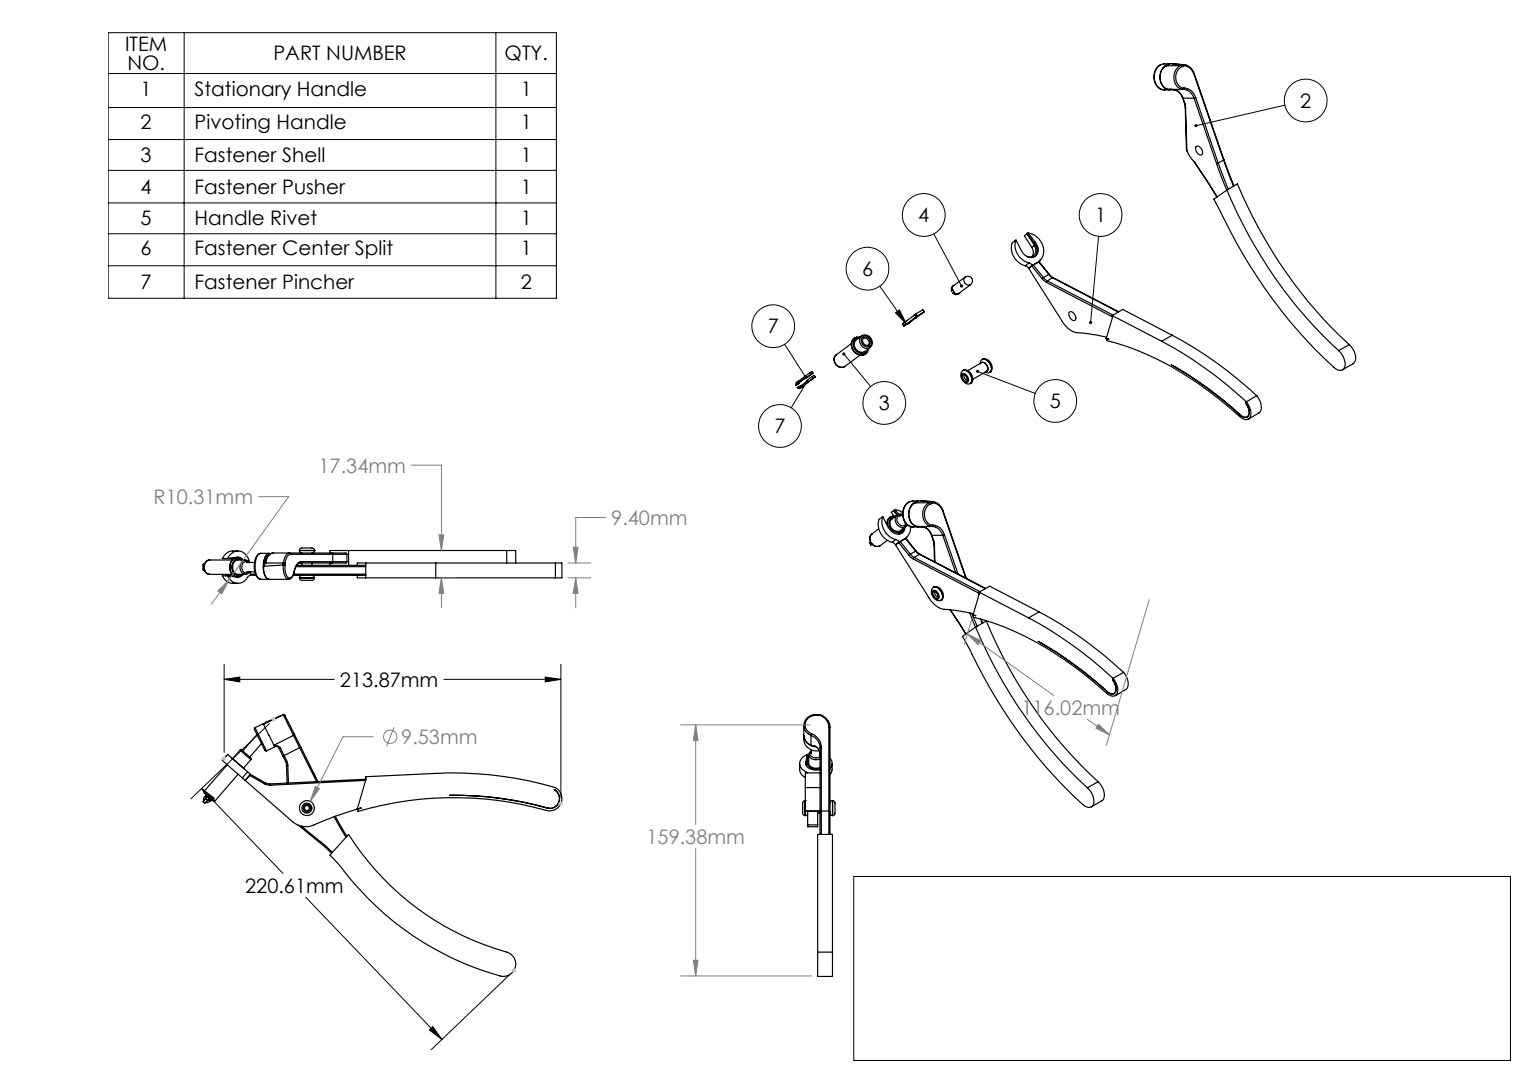
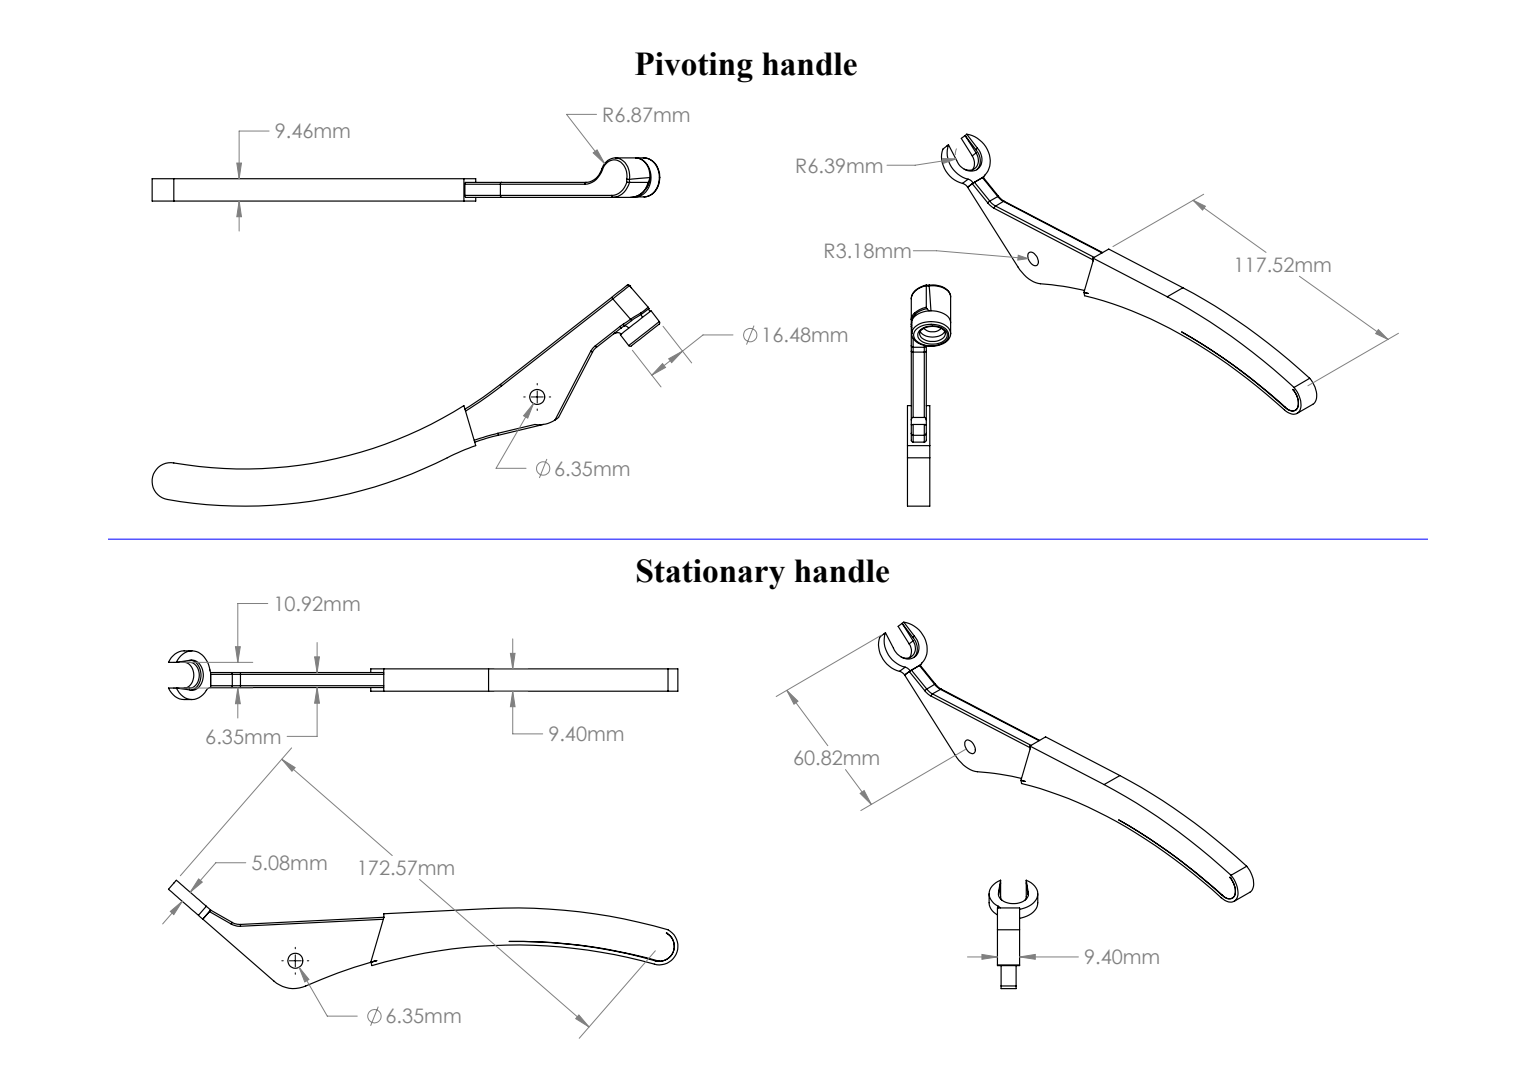
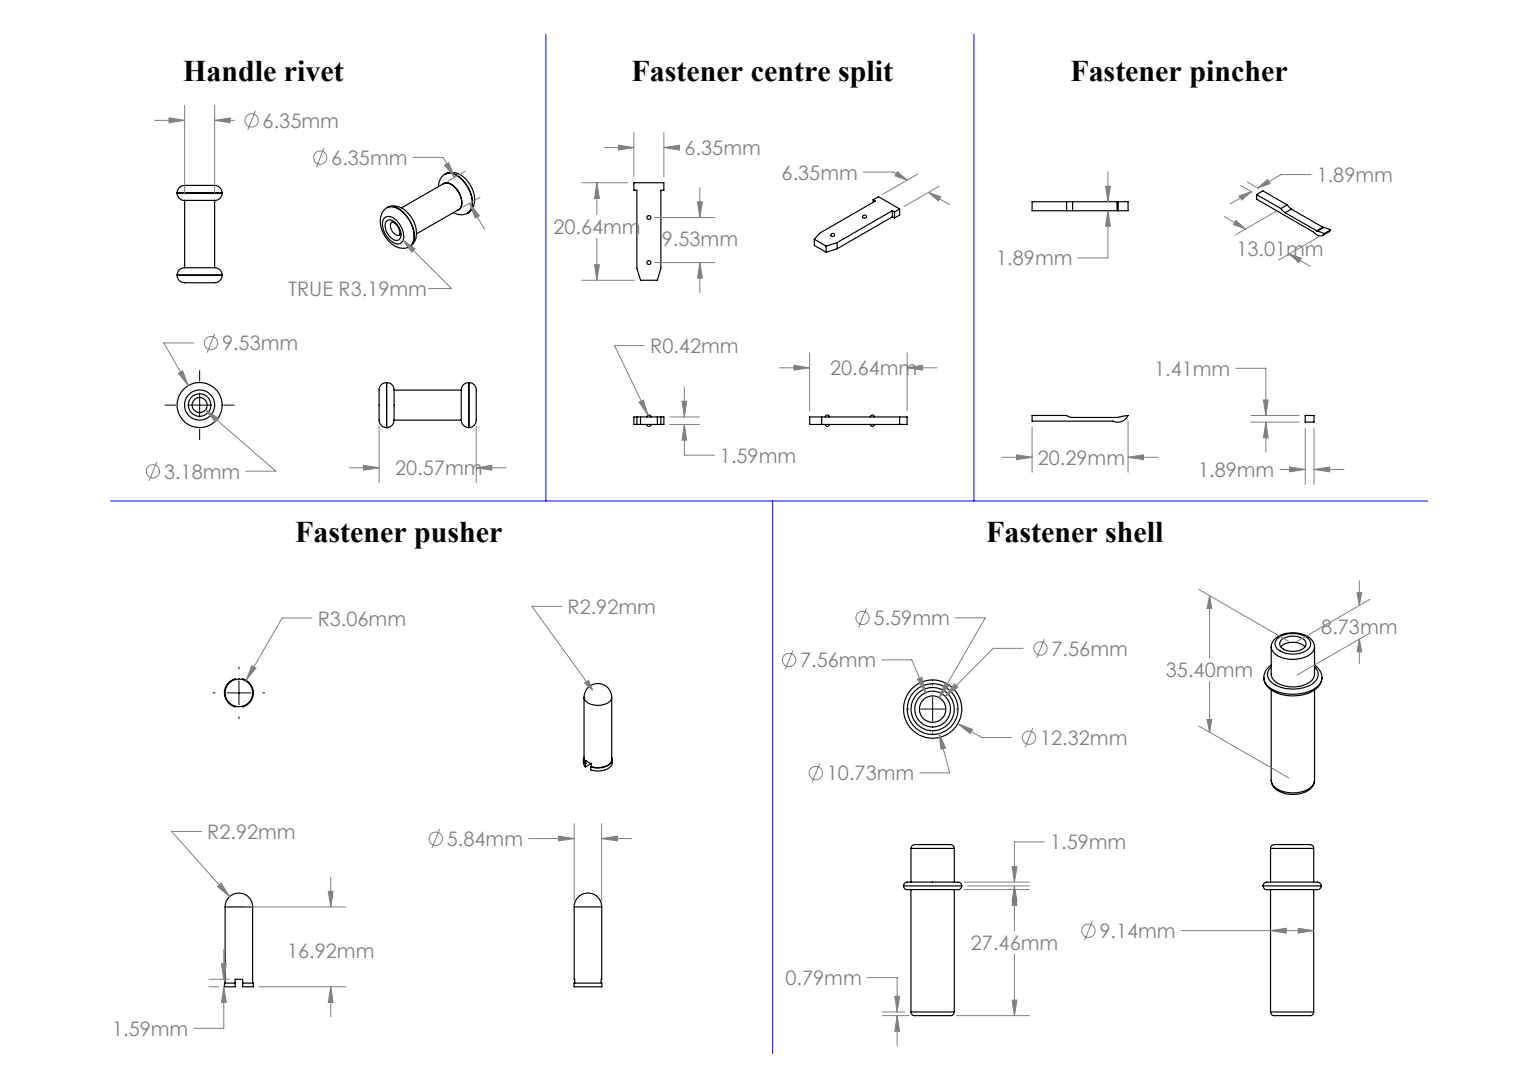
ISO-10303-21;
HEADER;
FILE_DESCRIPTION (('STEP AP203'),
    '1' );
FILE_NAME ('MAS-157',
    '2026-10-09T13:45:32',
    ( '' ),
    ( '' ),
    'SwSTEP 2.0',
    'SolidWorks 2024',
    '' );
FILE_SCHEMA (( 'AUTOMOTIVE_DESIGN' ));
ENDSEC;

DATA;
#1 = DIRECTION ( 'NONE',  ( -0.6157549048526801405, 0.7879377495398142139, 0.000000000000000000 ) ) ;
#2 = SHAPE_REPRESENTATION ( 'Cleco, Handle, Stationary', ( #3555 ), #5783 ) ;
#3 = DIRECTION ( 'NONE',  ( -1.000000000000000000, 0.000000000000000000, 0.000000000000000000 ) ) ;
#4 = ORIENTED_EDGE ( 'NONE', *, *, #5907, .T. ) ;
#5 = CARTESIAN_POINT ( 'NONE',  ( 1.850068364776406682, 1.494658567734585608, 0.000000000000000000 ) ) ;
#6 = VERTEX_POINT ( 'NONE', #7280 ) ;
#7 = LINE ( 'NONE', #8071, #3494 ) ;
#8 = PERSON_AND_ORGANIZATION ( #4735, #6190 ) ;
#9 = CARTESIAN_POINT ( 'NONE',  ( -5.996547682996108186, -1.882193845889704065, 0.2179999999999999993 ) ) ;
#10 = FACE_OUTER_BOUND ( 'NONE', #4917, .T. ) ;
#11 = EDGE_CURVE ( 'NONE', #2855, #2155, #1899, .T. ) ;
#12 = ORIENTED_EDGE ( 'NONE', *, *, #4444, .T. ) ;
#13 = FACE_OUTER_BOUND ( 'NONE', #2691, .T. ) ;
#14 = CARTESIAN_POINT ( 'NONE',  ( 0.6250000000000000000, -0.07812500000000001388, 0.000000000000000000 ) ) ;
#15 = DIRECTION ( 'NONE',  ( 1.000000000000000000, 8.970601940444434686E-12, 0.000000000000000000 ) ) ;
#16 = APPROVAL_DATE_TIME ( #593, #3996 ) ;
#17 = LINE ( 'NONE', #7477, #1803 ) ;
#18 = DIRECTION ( 'NONE',  ( 0.000000000000000000, 0.000000000000000000, -1.000000000000000000 ) ) ;
#19 = VERTEX_POINT ( 'NONE', #3930 ) ;
#20 = ORIENTED_EDGE ( 'NONE', *, *, #5646, .T. ) ;
#21 = EDGE_CURVE ( 'NONE', #2327, #24, #2891, .T. ) ;
#22 = EDGE_CURVE ( 'NONE', #963, #158, #1365, .T. ) ;
#23 = LOCAL_TIME ( 14, 45, 32.00000000000000000, #7946 ) ;
#24 = VERTEX_POINT ( 'NONE', #7323 ) ;
#25 = AXIS2_PLACEMENT_3D ( 'NONE', #111, #2600, #7606 ) ;
#26 = FACE_OUTER_BOUND ( 'NONE', #6824, .T. ) ;
#27 = CC_DESIGN_PERSON_AND_ORGANIZATION_ASSIGNMENT ( #2008, #749, ( #3335 ) ) ;
#28 = CARTESIAN_POINT ( 'NONE',  ( 1.416570667224800406, 1.056400084382879134, -0.2054632529226294024 ) ) ;
#29 = EDGE_CURVE ( 'NONE', #3273, #1544, #5158, .T. ) ;
#30 = LINE ( 'NONE', #3883, #1333 ) ;
#31 = ORIENTED_EDGE ( 'NONE', *, *, #3836, .F. ) ;
#32 = DIRECTION ( 'NONE',  ( -0.000000000000000000, 0.000000000000000000, 1.000000000000000000 ) ) ;
#33 = B_SPLINE_CURVE_WITH_KNOTS ( 'NONE', 3,
 ( #1903, #1397, #3941, #5831 ),
 .UNSPECIFIED., .F., .F.,
 ( 4, 4 ),
 ( 0.001688628934469491114, 0.002127673841090521080 ),
 .UNSPECIFIED. ) ;
#34 = VECTOR ( 'NONE', #5125, 39.37007874015748143 ) ;
#35 = CARTESIAN_POINT ( 'NONE',  ( -1.204376266962890796, -0.2040480809676099017, 0.2500000000000000000 ) ) ;
#36 = CARTESIAN_POINT ( 'NONE',  ( -1.763177565995708296, 1.070083551578370207, -0.08100000000000007194 ) ) ;
#37 = CALENDAR_DATE ( 2026, 9, 10 ) ;
#38 = ORIENTED_EDGE ( 'NONE', *, *, #6492, .T. ) ;
#39 = CIRCLE ( 'NONE', #5286, 0.06200000000000004813 ) ;
#40 = CARTESIAN_POINT ( 'NONE',  ( 1.323792169463187340, 1.088966521967518863, -0.1270528182937126493 ) ) ;
#41 = CARTESIAN_POINT ( 'NONE',  ( 0.000000000000000000, 0.6124999999999999334, 0.000000000000000000 ) ) ;
#42 = CARTESIAN_POINT ( 'NONE',  ( 1.684866161243239846, 1.178252195112418299, -0.1039999999999998703 ) ) ;
#43 = VECTOR ( 'NONE', #928, 39.37007874015748143 ) ;
#44 = CARTESIAN_POINT ( 'NONE',  ( -1.067641779222573639, 0.6107141540073635078, 0.09374999999999998612 ) ) ;
#45 = DIRECTION ( 'NONE',  ( 1.000000000000000000, 0.000000000000000000, 0.000000000000000000 ) ) ;
#46 = DIRECTION ( 'NONE',  ( -0.000000000000000000, -0.000000000000000000, -1.000000000000000000 ) ) ;
#47 = CARTESIAN_POINT ( 'NONE',  ( 0.000000000000000000, 0.6124999999999999334, 0.000000000000000000 ) ) ;
#48 = CIRCLE ( 'NONE', #181, 0.3547681700190749576 ) ;
#49 = AXIS2_PLACEMENT_3D ( 'NONE', #6623, #1014, #5431 ) ;
#50 = ORIENTED_EDGE ( 'NONE', *, *, #1216, .T. ) ;
#51 = SECURITY_CLASSIFICATION ( '', '', #1852 ) ;
#52 = CIRCLE ( 'NONE', #6609, 0.1875000000000000278 ) ;
#53 = EDGE_LOOP ( 'NONE', ( #7030, #861, #647, #7343 ) ) ;
#54 = DIRECTION ( 'NONE',  ( -0.000000000000000000, -0.000000000000000000, -1.000000000000000000 ) ) ;
#55 = DIRECTION ( 'NONE',  ( -1.000000000000000000, 0.000000000000000000, 0.000000000000000000 ) ) ;
#56 = MECHANICAL_CONTEXT ( 'NONE', #1115, 'mechanical' ) ;
#57 = CARTESIAN_POINT ( 'NONE',  ( 6.190221022838899856, 0.4584861219976859026, 0.1250000000000004441 ) ) ;
#58 = FACE_BOUND ( 'NONE', #2776, .T. ) ;
#59 = ORIENTED_EDGE ( 'NONE', *, *, #2335, .F. ) ;
#60 = VECTOR ( 'NONE', #178, 39.37007874015747433 ) ;
#61 = AXIS2_PLACEMENT_3D ( 'NONE', #3635, #4900, #4323 ) ;
#62 = DIRECTION ( 'NONE',  ( 0.8639477456102231390, 0.5035814659566147933, -0.000000000000000000 ) ) ;
#63 = CIRCLE ( 'NONE', #3353, 0.09999999999999999167 ) ;
#64 = CIRCLE ( 'NONE', #588, 0.1255000000000000282 ) ;
#65 = ORIENTED_EDGE ( 'NONE', *, *, #5052, .T. ) ;
#66 = FACE_OUTER_BOUND ( 'NONE', #5233, .T. ) ;
#67 = CYLINDRICAL_SURFACE ( 'NONE', #6771, 0.03124999999999999306 ) ;
#68 = EDGE_CURVE ( 'NONE', #5482, #3124, #1464, .T. ) ;
#69 = EDGE_CURVE ( 'NONE', #6638, #4615, #2677, .T. ) ;
#70 = CARTESIAN_POINT ( 'NONE',  ( 1.752412446118922995, 1.417229020394738415, 0.1726873346618605365 ) ) ;
#71 = ORIENTED_EDGE ( 'NONE', *, *, #7527, .T. ) ;
#72 = DIRECTION ( 'NONE',  ( 0.000000000000000000, 0.000000000000000000, -1.000000000000000000 ) ) ;
#73 = CIRCLE ( 'NONE', #5578, 0.2425000000000000211 ) ;
#74 = EDGE_CURVE ( 'NONE', #1061, #1984, #3077, .T. ) ;
#75 = ORIENTED_EDGE ( 'NONE', *, *, #993, .T. ) ;
#76 = FACE_OUTER_BOUND ( 'NONE', #4236, .T. ) ;
#77 = DIRECTION ( 'NONE',  ( -1.000000000000000000, 0.000000000000000000, 0.000000000000000000 ) ) ;
#78 = AXIS2_PLACEMENT_3D ( 'NONE', #1308, #3818, #6319 ) ;
#79 = APPLICATION_PROTOCOL_DEFINITION ( 'international standard', 'config_control_design', 1994, #1637 ) ;
#80 = EDGE_CURVE ( 'NONE', #1875, #4512, #6627, .T. ) ;
#81 = VERTEX_POINT ( 'NONE', #6665 ) ;
#82 = EDGE_CURVE ( 'NONE', #7062, #4072, #1053, .T. ) ;
#83 = DIRECTION ( 'NONE',  ( 0.000000000000000000, 0.000000000000000000, 1.000000000000000000 ) ) ;
#84 = DIRECTION ( 'NONE',  ( 0.7879377495398138809, 0.6157549048526804736, 0.000000000000000000 ) ) ;
#85 = EDGE_LOOP ( 'NONE', ( #926, #3795, #4009, #2620 ) ) ;
#86 = AXIS2_PLACEMENT_3D ( 'NONE', #7852, #2824, #5333 ) ;
#87 = DIRECTION ( 'NONE',  ( -0.6568496200222107007, -0.7540216022612863389, 0.000000000000000000 ) ) ;
#88 = AXIS2_PLACEMENT_3D ( 'NONE', #2138, #3280, #7015 ) ;
#89 = APPROVAL ( #7734, 'UNSPECIFIED' ) ;
#90 = EDGE_CURVE ( 'NONE', #3501, #7797, #7679, .T. ) ;
#91 = VERTEX_POINT ( 'NONE', #2513 ) ;
#92 = AXIS2_PLACEMENT_3D ( 'NONE', #7571, #6383, #766 ) ;
#93 = DIRECTION ( 'NONE',  ( 0.7879377495398159903, 0.6157549048526775870, -0.000000000000000000 ) ) ;
#94 = APPROVAL_ROLE ( '' ) ;
#95 = DIRECTION ( 'NONE',  ( 0.000000000000000000, 1.000000000000000000, 0.000000000000000000 ) ) ;
#96 = DATE_AND_TIME ( #5751, #4257 ) ;
#97 = CARTESIAN_POINT ( 'NONE',  ( 0.000000000000000000, 0.03124999999999997571, 0.000000000000000000 ) ) ;
#98 = CIRCLE ( 'NONE', #4156, 6.962657474112426748 ) ;
#99 = ORIENTED_EDGE ( 'NONE', *, *, #6424, .F. ) ;
#100 = AXIS2_PLACEMENT_3D ( 'NONE', #6028, #4066, #402 ) ;
#101 = FACE_OUTER_BOUND ( 'NONE', #53, .T. ) ;
#102 = PERSON_AND_ORGANIZATION ( #4735, #6190 ) ;
#103 = CARTESIAN_POINT ( 'NONE',  ( -0.1250000000000000000, 1.530808498934191509E-17, -0.5599999999999999423 ) ) ;
#104 = DIRECTION ( 'NONE',  ( 1.821231995776175479E-16, 1.000000000000000000, 0.000000000000000000 ) ) ;
#105 = ORIENTED_EDGE ( 'NONE', *, *, #272, .F. ) ;
#106 = ORIENTED_EDGE ( 'NONE', *, *, #2026, .T. ) ;
#107 = FACE_OUTER_BOUND ( 'NONE', #1359, .T. ) ;
#108 = ORIENTED_EDGE ( 'NONE', *, *, #7591, .T. ) ;
#109 = CARTESIAN_POINT ( 'NONE',  ( 0.000000000000000000, 0.000000000000000000, 0.2500000000000000000 ) ) ;
#110 = CARTESIAN_POINT ( 'NONE',  ( 1.417684048173985634, 1.054372030571947283, -0.2033754655707550874 ) ) ;
#111 = CARTESIAN_POINT ( 'NONE',  ( 0.000000000000000000, 0.000000000000000000, 0.2500000000000000000 ) ) ;
#112 = VERTEX_POINT ( 'NONE', #7478 ) ;
#113 = DIRECTION ( 'NONE',  ( 0.000000000000000000, 0.000000000000000000, -1.000000000000000000 ) ) ;
#114 = ORIENTED_EDGE ( 'NONE', *, *, #7639, .F. ) ;
#115 = CARTESIAN_POINT ( 'NONE',  ( 1.832772415705825830, 1.448773774648827617, 0.06821617062301892076 ) ) ;
#116 = DIRECTION ( 'NONE',  ( 1.000000000000000000, -0.000000000000000000, -0.000000000000000000 ) ) ;
#117 = DATE_AND_TIME ( #5742, #3955 ) ;
#118 = ORIENTED_EDGE ( 'NONE', *, *, #4536, .T. ) ;
#119 = DIRECTION ( 'NONE',  ( 0.000000000000000000, 0.000000000000000000, -1.000000000000000000 ) ) ;
#120 = CARTESIAN_POINT ( 'NONE',  ( 1.380988422957101003, 1.174934410393058126, 0.2179999999999999993 ) ) ;
#121 = ORIENTED_EDGE ( 'NONE', *, *, #1777, .F. ) ;
#122 = DIRECTION ( 'NONE',  ( 0.7540216022612864499, -0.6568496200222104786, 0.000000000000000000 ) ) ;
#123 = EDGE_CURVE ( 'NONE', #4974, #3239, #3718, .T. ) ;
#124 = ADVANCED_FACE ( 'NONE', ( #549 ), #7584, .F. ) ;
#125 = EDGE_CURVE ( 'NONE', #2487, #1575, #5560, .T. ) ;
#126 = EDGE_CURVE ( 'NONE', #3812, #6, #587, .T. ) ;
#127 =( CONVERSION_BASED_UNIT ( 'INCH', #2499 ) LENGTH_UNIT ( ) NAMED_UNIT ( #5631 ) );
#128 = DIRECTION ( 'NONE',  ( -0.000000000000000000, 1.000000000000000000, -0.000000000000000000 ) ) ;
#129 = ORIENTED_EDGE ( 'NONE', *, *, #6348, .F. ) ;
#130 = CARTESIAN_POINT ( 'NONE',  ( 1.531818848064314453, 1.858671604592519344, -3.087930470258342319E-05 ) ) ;
#131 = EDGE_CURVE ( 'NONE', #668, #4233, #6788, .T. ) ;
#132 = DIRECTION ( 'NONE',  ( 0.000000000000000000, 0.000000000000000000, 1.000000000000000000 ) ) ;
#133 = EDGE_CURVE ( 'NONE', #2990, #3476, #3761, .T. ) ;
#134 = ORIENTED_EDGE ( 'NONE', *, *, #3394, .F. ) ;
#135 = DIRECTION ( 'NONE',  ( 1.000000000000000000, 0.000000000000000000, 0.000000000000000000 ) ) ;
#136 = CARTESIAN_POINT ( 'NONE',  ( 1.723350842796532278, 1.129006085766179890, -0.1039999999999998703 ) ) ;
#137 = COORDINATED_UNIVERSAL_TIME_OFFSET ( 0, 0, .AHEAD. ) ;
#138 = DIRECTION ( 'NONE',  ( -0.4606913525677313603, -0.8875604078987042733, -0.000000000000000000 ) ) ;
#139 = DIRECTION ( 'NONE',  ( -0.000000000000000000, 0.000000000000000000, 1.000000000000000000 ) ) ;
#140 = VERTEX_POINT ( 'NONE', #3018 ) ;
#141 = VERTEX_POINT ( 'NONE', #7361 ) ;
#142 = EDGE_LOOP ( 'NONE', ( #3147, #7500, #5095 ) ) ;
#143 = FACE_OUTER_BOUND ( 'NONE', #230, .T. ) ;
#144 = APPROVAL_PERSON_ORGANIZATION ( #7760, #2585, #5389 ) ;
#145 = EDGE_LOOP ( 'NONE', ( #637, #5534, #4273, #3035, #377, #5498, #741, #1949, #1567, #4620 ) ) ;
#146 = DIRECTION ( 'NONE',  ( -0.04906492035527518919, 0.9987955914953422498, 0.000000000000000000 ) ) ;
#147 = CARTESIAN_POINT ( 'NONE',  ( 0.2896281645421511231, -0.04777128394798136474, 0.07449999999999999678 ) ) ;
#148 = CARTESIAN_POINT ( 'NONE',  ( -0.1250000000000000000, 0.5625000000000000000, 0.03125000000000000000 ) ) ;
#149 = CARTESIAN_POINT ( 'NONE',  ( 0.1250000000000000000, 0.000000000000000000, -0.5599999999999999423 ) ) ;
#150 = LOCAL_TIME ( 14, 45, 32.00000000000000000, #1109 ) ;
#151 = EDGE_LOOP ( 'NONE', ( #4432, #6165, #5491, #6432 ) ) ;
#152 = CARTESIAN_POINT ( 'NONE',  ( 1.792094459600980905, 1.446946837835136890, 0.1263687957420392971 ) ) ;
#153 = DIRECTION ( 'NONE',  ( -0.000000000000000000, -1.000000000000000000, -0.000000000000000000 ) ) ;
#154 = PERSON_AND_ORGANIZATION ( #4735, #6190 ) ;
#155 = ORIENTED_EDGE ( 'NONE', *, *, #2026, .F. ) ;
#156 = CARTESIAN_POINT ( 'NONE',  ( -4.882388066182508091, 5.670153330992292240, 0.000000000000000000 ) ) ;
#157 = FACE_OUTER_BOUND ( 'NONE', #262, .T. ) ;
#158 = VERTEX_POINT ( 'NONE', #6270 ) ;
#159 = CIRCLE ( 'NONE', #7494, 0.1255000000000000282 ) ;
#160 = FACE_OUTER_BOUND ( 'NONE', #466, .T. ) ;
#161 = AXIS2_PLACEMENT_3D ( 'NONE', #1394, #5055, #7509 ) ;
#162 = CC_DESIGN_SECURITY_CLASSIFICATION ( #7233, ( #4480 ) ) ;
#163 = TOROIDAL_SURFACE ( 'NONE', #1468, 0.1255000000000000282, 0.06199999999999999956 ) ;
#164 = DIRECTION ( 'NONE',  ( -0.000000000000000000, -0.000000000000000000, -1.000000000000000000 ) ) ;
#165 = CARTESIAN_POINT ( 'NONE',  ( 0.000000000000000000, 1.112500000000000044, 0.2112499999999999933 ) ) ;
#166 = DIRECTION ( 'NONE',  ( -8.441663814850087926E-16, -1.362795760884335707E-15, 1.000000000000000000 ) ) ;
#167 = LINE ( 'NONE', #5090, #7384 ) ;
#168 = EDGE_CURVE ( 'NONE', #5062, #1238, #991, .T. ) ;
#169 = DIRECTION ( 'NONE',  ( -0.6157549048526804736, 0.7879377495398138809, 0.000000000000000000 ) ) ;
#170 = EDGE_CURVE ( 'NONE', #2750, #4309, #1294, .T. ) ;
#171 = CARTESIAN_POINT ( 'NONE',  ( -0.1054677083281892608, 0.6124999999999999334, 0.03125000000000000000 ) ) ;
#172 = PRODUCT_DEFINITION ( 'UNKNOWN', '', #7483, #3514 ) ;
#173 = DIRECTION ( 'NONE',  ( -0.000000000000000000, -0.000000000000000000, -1.000000000000000000 ) ) ;
#174 = AXIS2_PLACEMENT_3D ( 'NONE', #7286, #2325, #6791 ) ;
#175 = DIRECTION ( 'NONE',  ( -0.6157549048526804736, 0.7879377495398138809, -0.000000000000000000 ) ) ;
#176 = APPROVAL_ROLE ( '' ) ;
#177 = LINE ( 'NONE', #220, #2975 ) ;
#178 = DIRECTION ( 'NONE',  ( -0.7879377495398141029, -0.6157549048526802515, 0.000000000000000000 ) ) ;
#179 = ADVANCED_FACE ( 'NONE', ( #8043 ), #2438, .T. ) ;
#180 = ORIENTED_EDGE ( 'NONE', *, *, #3278, .F. ) ;
#181 = AXIS2_PLACEMENT_3D ( 'NONE', #5513, #3140, #511 ) ;
#182 = ORIENTED_EDGE ( 'NONE', *, *, #8026, .T. ) ;
#183 = CARTESIAN_POINT ( 'NONE',  ( 1.437142212821869380, 1.212327995214701915, 0.2179999999999999993 ) ) ;
#184 = EDGE_LOOP ( 'NONE', ( #3311, #1599, #1452, #4954 ) ) ;
#185 = CARTESIAN_POINT ( 'NONE',  ( 1.584081668904965046, 1.313867407547560484, 0.2488142415425237675 ) ) ;
#186 = LINE ( 'NONE', #1255, #214 ) ;
#187 = SECURITY_CLASSIFICATION ( '', '', #6292 ) ;
#188 = CIRCLE ( 'NONE', #3205, 0.1250000000000000000 ) ;
#189 = FACE_OUTER_BOUND ( 'NONE', #317, .T. ) ;
#190 = CARTESIAN_POINT ( 'NONE',  ( 1.258616367985684104, -0.02482036785324303815, 0.1849999999999999978 ) ) ;
#191 = CLOSED_SHELL ( 'NONE', ( #5192, #6881, #1622, #3884, #1222, #3083, #341, #2322, #4646, #2841, #3828, #5309, #3477, #3646, #3790, #635, #4984, #179, #5486, #4337, #4696, #6894, #4687, #1314, #3240, #2939, #7837, #1030, #6205, #3651, #6792, #6797, #4635, #2616, #2625, #3329, #3092, #621, #3082, #5243, #4004, #437, #7292, #1593, #3238, #5295, #4287, #7493, #7092, #5494, #2033, #4935, #4584, #5121, #4592, #5599, #6682, #1830, #4404, #124, #5528, #1872, #6303, #7451, #4098, #414 ) ) ;
#192 = AXIS2_PLACEMENT_3D ( 'NONE', #3731, #7460, #6925 ) ;
#193 = EDGE_LOOP ( 'NONE', ( #7590, #4456, #4395, #5162 ) ) ;
#194 = CARTESIAN_POINT ( 'NONE',  ( 1.477881298880768357, 1.805595895546355356, 0.1305532412730666392 ) ) ;
#195 = CARTESIAN_POINT ( 'NONE',  ( 4.013019369095008670, -4.147396371033809537, 0.1250000000000000000 ) ) ;
#196 = COORDINATED_UNIVERSAL_TIME_OFFSET ( 0, 0, .AHEAD. ) ;
#197 = CARTESIAN_POINT ( 'NONE',  ( -0.03125000000000000000, -0.03125000000000000000, -0.1162848326531996102 ) ) ;
#198 = DIRECTION ( 'NONE',  ( 0.000000000000000000, 0.000000000000000000, -1.000000000000000000 ) ) ;
#199 = CARTESIAN_POINT ( 'NONE',  ( 0.2796912674003787513, -4.528516545235624413, 0.000000000000000000 ) ) ;
#200 = TOROIDAL_SURFACE ( 'NONE', #2550, 0.2468203157102362433, 0.03200000000000000067 ) ;
#201 = ORIENTED_EDGE ( 'NONE', *, *, #4988, .T. ) ;
#202 = DIRECTION ( 'NONE',  ( -0.8680936205257663296, 0.4964005096718443477, -0.000000000000000000 ) ) ;
#203 = AXIS2_PLACEMENT_3D ( 'NONE', #6124, #1765, #1112 ) ;
#204 = DIRECTION ( 'NONE',  ( 0.000000000000000000, 1.000000000000000000, 0.000000000000000000 ) ) ;
#205 = CARTESIAN_POINT ( 'NONE',  ( -1.983451234524918227, 1.341543513548240529, 0.1339999999999995917 ) ) ;
#206 = DATE_AND_TIME ( #3327, #7872 ) ;
#207 = ORIENTED_EDGE ( 'NONE', *, *, #5593, .T. ) ;
#208 = CIRCLE ( 'NONE', #7670, 0.2515937209583817280 ) ;
#209 = ORIENTED_EDGE ( 'NONE', *, *, #2574, .T. ) ;
#210 = VECTOR ( 'NONE', #4441, 39.37007874015748143 ) ;
#211 = DIRECTION ( 'NONE',  ( 0.000000000000000000, 1.000000000000000000, -0.000000000000000000 ) ) ;
#212 = CARTESIAN_POINT ( 'NONE',  ( 0.000000000000000000, 0.000000000000000000, 0.000000000000000000 ) ) ;
#213 = VECTOR ( 'NONE', #4099, 39.37007874015748143 ) ;
#214 = VECTOR ( 'NONE', #2035, 39.37007874015748143 ) ;
#215 = EDGE_CURVE ( 'NONE', #5845, #2895, #393, .T. ) ;
#216 = ORIENTED_EDGE ( 'NONE', *, *, #4390, .T. ) ;
#217 = DIRECTION ( 'NONE',  ( -0.000000000000000000, -1.000000000000000000, -0.000000000000000000 ) ) ;
#218 = DIRECTION ( 'NONE',  ( 0.6157549048526804736, -0.7879377495398138809, -0.000000000000000000 ) ) ;
#219 = PERSON_AND_ORGANIZATION_ROLE ( 'design_supplier' ) ;
#220 = CARTESIAN_POINT ( 'NONE',  ( -1.803041671366327314, 1.104810305277056592, 0.1649762307749162715 ) ) ;
#221 = DIRECTION ( 'NONE',  ( 0.000000000000000000, 1.000000000000000000, 0.000000000000000000 ) ) ;
#222 = ORIENTED_EDGE ( 'NONE', *, *, #3824, .T. ) ;
#223 = VECTOR ( 'NONE', #4254, 39.37007874015748143 ) ;
#224 = VECTOR ( 'NONE', #4772, 39.37007874015748143 ) ;
#225 = VERTEX_POINT ( 'NONE', #7448 ) ;
#226 = ADVANCED_FACE ( 'NONE', ( #1827 ), #5682, .F. ) ;
#227 = VECTOR ( 'NONE', #2539, 39.37007874015748143 ) ;
#228 = ORIENTED_EDGE ( 'NONE', *, *, #6845, .T. ) ;
#229 = CARTESIAN_POINT ( 'NONE',  ( 0.000000000000000000, 0.6124999999999999334, 0.000000000000000000 ) ) ;
#230 = EDGE_LOOP ( 'NONE', ( #2845, #7874, #3535, #5828 ) ) ;
#231 = EDGE_CURVE ( 'NONE', #1921, #3782, #676, .T. ) ;
#232 = CARTESIAN_POINT ( 'NONE',  ( 1.731490805950789191, 1.384744806415751484, 0.1971537411645175319 ) ) ;
#233 = LINE ( 'NONE', #1455, #4810 ) ;
#234 = CC_DESIGN_PERSON_AND_ORGANIZATION_ASSIGNMENT ( #6677, #1065, ( #7731 ) ) ;
#235 = DIRECTION ( 'NONE',  ( 0.000000000000000000, 0.000000000000000000, -1.000000000000000000 ) ) ;
#236 = EDGE_CURVE ( 'NONE', #2236, #880, #3736, .T. ) ;
#237 = DIRECTION ( 'NONE',  ( -1.000000000000000000, 0.000000000000000000, 0.000000000000000000 ) ) ;
#238 = PERSON ( 'NAUO-PER3', 'UNSPECIFIED', 'UNSPECIFIED', ('UNSPECIFIED'), ('UNSPECIFIED'), ('UNSPECIFIED') ) ;
#239 = ORIENTED_EDGE ( 'NONE', *, *, #131, .T. ) ;
#240 = ORIENTED_EDGE ( 'NONE', *, *, #562, .T. ) ;
#241 = CARTESIAN_POINT ( 'NONE',  ( 1.296168929684020199, 1.702605512879020955, 0.2124775937629295175 ) ) ;
#242 = DIRECTION ( 'NONE',  ( -0.000000000000000000, -1.000000000000000000, -0.000000000000000000 ) ) ;
#243 = CALENDAR_DATE ( 2026, 9, 10 ) ;
#244 = ORIENTED_EDGE ( 'NONE', *, *, #7043, .T. ) ;
#245 = CARTESIAN_POINT ( 'NONE',  ( 2.387087291339119677, -6.013863021948615106, 0.1250000000000000000 ) ) ;
#246 = LINE ( 'NONE', #7853, #7674 ) ;
#247 = EDGE_LOOP ( 'NONE', ( #7423, #3661, #721, #3628 ) ) ;
#248 = PLANE ( 'NONE',  #4227 ) ;
#249 = CARTESIAN_POINT ( 'NONE',  ( 0.2896281645421511231, -0.04777128394798136474, 0.07449999999999999678 ) ) ;
#250 = DIRECTION ( 'NONE',  ( -0.000000000000000000, -0.000000000000000000, 1.000000000000000000 ) ) ;
#251 = DATE_AND_TIME ( #3490, #7738 ) ;
#252 = ORIENTED_EDGE ( 'NONE', *, *, #2079, .F. ) ;
#253 = CARTESIAN_POINT ( 'NONE',  ( 0.3566525292043903339, -0.3408511508279103985, 0.2179999999999999993 ) ) ;
#254 = CARTESIAN_POINT ( 'NONE',  ( 1.556400554713971651, 1.293514327272109687, 0.2500000000000000000 ) ) ;
#255 = VERTEX_POINT ( 'NONE', #1363 ) ;
#256 = ORIENTED_EDGE ( 'NONE', *, *, #330, .T. ) ;
#257 = CARTESIAN_POINT ( 'NONE',  ( 0.000000000000000000, 0.03125000000000000000, 0.000000000000000000 ) ) ;
#258 = CARTESIAN_POINT ( 'NONE',  ( -1.693021742871659407, 0.8232980029552862122, -0.08100000000000007194 ) ) ;
#259 = COORDINATED_UNIVERSAL_TIME_OFFSET ( 0, 0, .AHEAD. ) ;
#260 = CARTESIAN_POINT ( 'NONE',  ( -6.420602001755994159, -1.404684638105634820, 0.3125000000000000000 ) ) ;
#261 = DIRECTION ( 'NONE',  ( -0.6157549048526801405, 0.7879377495398141029, 0.000000000000000000 ) ) ;
#262 = EDGE_LOOP ( 'NONE', ( #7569, #4120, #399, #6373 ) ) ;
#263 = EDGE_LOOP ( 'NONE', ( #2370, #5104, #2202, #5817, #4197, #6775 ) ) ;
#264 = ORIENTED_EDGE ( 'NONE', *, *, #6391, .T. ) ;
#265 = LINE ( 'NONE', #2764, #712 ) ;
#266 = ORIENTED_EDGE ( 'NONE', *, *, #7875, .T. ) ;
#267 = DIRECTION ( 'NONE',  ( 1.000000000000000000, 0.000000000000000000, 0.000000000000000000 ) ) ;
#268 = DIRECTION ( 'NONE',  ( 1.000000000000000000, 4.484396833652621360E-12, 0.000000000000000000 ) ) ;
#269 = CARTESIAN_POINT ( 'NONE',  ( 6.067385397437120353, 0.2407432673787524013, -0.1849999999999999978 ) ) ;
#270 = EDGE_CURVE ( 'NONE', #5976, #1875, #3258, .T. ) ;
#271 = EDGE_LOOP ( 'NONE', ( #4082, #3585, #738, #5261 ) ) ;
#272 = EDGE_CURVE ( 'NONE', #2232, #1125, #6871, .T. ) ;
#273 = CARTESIAN_POINT ( 'NONE',  ( 0.9887166869077884668, 0.8277708867933829540, 0.2179999999999999993 ) ) ;
#274 = ORIENTED_EDGE ( 'NONE', *, *, #3349, .T. ) ;
#275 =( REPRESENTATION_RELATIONSHIP ('NONE','NONE', #3360, #2 ) REPRESENTATION_RELATIONSHIP_WITH_TRANSFORMATION ( #6984 )SHAPE_REPRESENTATION_RELATIONSHIP( ) );
#276 = ORIENTED_EDGE ( 'NONE', *, *, #636, .F. ) ;
#277 = EDGE_CURVE ( 'NONE', #2657, #19, #2545, .T. ) ;
#278 = PRODUCT_DEFINITION_SHAPE ( 'NONE', 'NONE',  #8095 ) ;
#279 = CARTESIAN_POINT ( 'NONE',  ( 1.806702786482898393, 1.440892520688004552, 0.1183513045165567601 ) ) ;
#280 = EDGE_CURVE ( 'NONE', #7184, #7717, #6454, .T. ) ;
#281 = DIRECTION ( 'NONE',  ( -0.000000000000000000, -0.000000000000000000, -1.000000000000000000 ) ) ;
#282 = PERSON_AND_ORGANIZATION ( #4735, #6190 ) ;
#283 = FACE_OUTER_BOUND ( 'NONE', #2655, .T. ) ;
#284 = CARTESIAN_POINT ( 'NONE',  ( 3.659299226295303686, -8.245510427152350275, 5.393636709996481038 ) ) ;
#285 = EDGE_LOOP ( 'NONE', ( #3269, #3510 ) ) ;
#286 = CARTESIAN_POINT ( 'NONE',  ( -0.09374999999999998612, 0.000000000000000000, -0.6537499999999999423 ) ) ;
#287 = LOCAL_TIME ( 14, 45, 32.00000000000000000, #7541 ) ;
#288 = CARTESIAN_POINT ( 'NONE',  ( 0.000000000000000000, 0.000000000000000000, 0.000000000000000000 ) ) ;
#289 = CARTESIAN_POINT ( 'NONE',  ( 1.475891671935536609, 0.7226544316391477762, 0.09374999999999998612 ) ) ;
#290 = APPROVAL_DATE_TIME ( #206, #1278 ) ;
#291 = ORIENTED_EDGE ( 'NONE', *, *, #4442, .F. ) ;
#292 = AXIS2_PLACEMENT_3D ( 'NONE', #5652, #7572, #690 ) ;
#293 = CARTESIAN_POINT ( 'NONE',  ( 1.490755817305508879, 1.854670610081086579, -0.01917321476376811912 ) ) ;
#294 = AXIS2_PLACEMENT_3D ( 'NONE', #5089, #3863, #4359 ) ;
#295 = APPROVAL_PERSON_ORGANIZATION ( #5514, #4698, #6098 ) ;
#296 = CIRCLE ( 'NONE', #818, 0.2819999999999998619 ) ;
#297 = VERTEX_POINT ( 'NONE', #794 ) ;
#298 = ORIENTED_EDGE ( 'NONE', *, *, #2680, .T. ) ;
#299 = FACE_OUTER_BOUND ( 'NONE', #4719, .T. ) ;
#300 = CARTESIAN_POINT ( 'NONE',  ( -0.09999999999999997780, 0.03125000000000000000, 0.7124999999999989120 ) ) ;
#301 = DATE_AND_TIME ( #968, #1894 ) ;
#302 = CARTESIAN_POINT ( 'NONE',  ( 1.855589205864664581, 1.487096013276917539, -0.0009044316923897459349 ) ) ;
#303 = AXIS2_PLACEMENT_3D ( 'NONE', #6878, #2039, #2570 ) ;
#304 = EDGE_LOOP ( 'NONE', ( #7542, #4529, #3682, #1925 ) ) ;
#305 = VERTEX_POINT ( 'NONE', #7109 ) ;
#306 = TOROIDAL_SURFACE ( 'NONE', #2004, 0.2819999999999999729, 0.03200000000000000067 ) ;
#307 = CARTESIAN_POINT ( 'NONE',  ( 1.347111479062088626E-17, 0.6124999999999999334, -0.1100000000000000006 ) ) ;
#308 = DESIGN_CONTEXT ( 'detailed design', #2518, 'design' ) ;
#309 = ORIENTED_EDGE ( 'NONE', *, *, #5941, .T. ) ;
#310 = DIRECTION ( 'NONE',  ( -1.000000000000000000, -9.329293658944590640E-14, 0.000000000000000000 ) ) ;
#311 = FACE_OUTER_BOUND ( 'NONE', #5756, .T. ) ;
#312 = CARTESIAN_POINT ( 'NONE',  ( 0.000000000000000000, 0.000000000000000000, -0.6219999999999999973 ) ) ;
#313 = AXIS2_PLACEMENT_3D ( 'NONE', #3150, #5649, #2520 ) ;
#314 = AXIS2_PLACEMENT_3D ( 'NONE', #9, #2546, #7556 ) ;
#315 = CARTESIAN_POINT ( 'NONE',  ( 1.283086085828156087, 1.692381576688154032, -0.1039999999999998703 ) ) ;
#316 = ORIENTED_EDGE ( 'NONE', *, *, #3989, .T. ) ;
#317 = EDGE_LOOP ( 'NONE', ( #5721, #5705, #2017, #5490 ) ) ;
#318 = LOCAL_TIME ( 14, 45, 32.00000000000000000, #3540 ) ;
#319 = ADVANCED_FACE ( 'NONE', ( #58, #837 ), #2558, .F. ) ;
#320 = CIRCLE ( 'NONE', #6999, 0.06249999999999995143 ) ;
#321 = CARTESIAN_POINT ( 'NONE',  ( 1.084347339223417528, 1.496459553539972287, -0.2249973011472257700 ) ) ;
#322 = DIRECTION ( 'NONE',  ( 0.6157549048526804736, -0.7879377495398138809, -0.000000000000000000 ) ) ;
#323 = CARTESIAN_POINT ( 'NONE',  ( 1.475891671935536609, 0.7226544316391472211, 0.1850000000000003586 ) ) ;
#324 = EDGE_LOOP ( 'NONE', ( #5970, #4767, #1019, #404 ) ) ;
#325 = DIRECTION ( 'NONE',  ( -0.9456454288325600865, 0.000000000000000000, -0.3251995124966879924 ) ) ;
#326 = CLOSED_SHELL ( 'NONE', ( #7293, #1213, #3576, #4699, #7146, #6554, #2083, #770, #1669, #5653, #4136, #4983, #4649, #2467, #682, #1691, #1876, #5950, #2226, #888, #6147, #4446, #7935, #563 ) ) ;
#327 = AXIS2_PLACEMENT_3D ( 'NONE', #1187, #5657, #7420 ) ;
#328 = EDGE_CURVE ( 'NONE', #7642, #4233, #2164, .T. ) ;
#329 = EDGE_CURVE ( 'NONE', #6037, #2842, #7011, .T. ) ;
#330 = EDGE_CURVE ( 'NONE', #6252, #7690, #7566, .T. ) ;
#331 = DIRECTION ( 'NONE',  ( 0.000000000000000000, -0.000000000000000000, -1.000000000000000000 ) ) ;
#332 = DIRECTION ( 'NONE',  ( -1.000000000000000000, 0.000000000000000000, 0.000000000000000000 ) ) ;
#333 = VECTOR ( 'NONE', #2009, 39.37007874015748143 ) ;
#334 = DATE_TIME_ROLE ( 'creation_date' ) ;
#335 = ORIENTED_EDGE ( 'NONE', *, *, #3688, .F. ) ;
#336 = EDGE_CURVE ( 'NONE', #6943, #6563, #5437, .T. ) ;
#337 = CARTESIAN_POINT ( 'NONE',  ( 0.3210248607526589026, -0.3692027715755950013, 0.2472403127172056181 ) ) ;
#338 = CARTESIAN_POINT ( 'NONE',  ( 0.1028096983035134415, -0.4582465879184300372, 0.2500000000000000000 ) ) ;
#339 = CC_DESIGN_PERSON_AND_ORGANIZATION_ASSIGNMENT ( #5182, #3341, ( #1471 ) ) ;
#340 = VERTEX_POINT ( 'NONE', #1324 ) ;
#341 = ADVANCED_FACE ( 'NONE', ( #7683 ), #200, .T. ) ;
#342 = CIRCLE ( 'NONE', #2559, 0.1250000000000000000 ) ;
#343 = ORIENTED_EDGE ( 'NONE', *, *, #3532, .F. ) ;
#344 = CIRCLE ( 'NONE', #5453, 0.1100000000000000006 ) ;
#345 = LENGTH_MEASURE_WITH_UNIT ( LENGTH_MEASURE( 0.02539999999999999897 ), #1907 );
#346 = ORIENTED_EDGE ( 'NONE', *, *, #7938, .F. ) ;
#347 = DIRECTION ( 'NONE',  ( -0.000000000000000000, -1.000000000000000000, -0.000000000000000000 ) ) ;
#348 = CARTESIAN_POINT ( 'NONE',  ( -0.1250000000000000000, 0.5625000000000000000, -0.03125000000000000000 ) ) ;
#349 = ITEM_DEFINED_TRANSFORMATION ( 'NONE', 'NONE', #161,  #3555 ) ;
#350 = CARTESIAN_POINT ( 'NONE',  ( 15385.85750733448185, -19684.85311172583170, -0.1039999999999998703 ) ) ;
#351 = CIRCLE ( 'NONE', #2179, 0.2468203157102362155 ) ;
#352 = ORIENTED_EDGE ( 'NONE', *, *, #4135, .T. ) ;
#353 = VERTEX_POINT ( 'NONE', #6414 ) ;
#354 = AXIS2_PLACEMENT_3D ( 'NONE', #4407, #5668, #4282 ) ;
#355 = LINE ( 'NONE', #2313, #3850 ) ;
#357 = CARTESIAN_POINT ( 'NONE',  ( 1.564847234473322191, 1.084460213605131562, -0.1039999999999998287 ) ) ;
#356 = AXIS2_PLACEMENT_3D ( 'NONE', #3356, #3430, #938 ) ;
#358 = VERTEX_POINT ( 'NONE', #3220 ) ;
#359 = CARTESIAN_POINT ( 'NONE',  ( 2.056298385200680201, 0.7198786976815826355, 0.09374999999999998612 ) ) ;
#360 = CARTESIAN_POINT ( 'NONE',  ( 1.821662113731687560E-17, 0.03125000000000000000, 0.1487499999999999933 ) ) ;
#361 = AXIS2_PLACEMENT_3D ( 'NONE', #4371, #138, #1976 ) ;
#362 = CYLINDRICAL_SURFACE ( 'NONE', #4659, 6.930657474112426719 ) ;
#363 = CARTESIAN_POINT ( 'NONE',  ( 0.000000000000000000, 0.03125000000000000000, 0.2896281645421511231 ) ) ;
#364 = LINE ( 'NONE', #3318, #4668 ) ;
#365 = VERTEX_POINT ( 'NONE', #2023 ) ;
#366 = DIRECTION ( 'NONE',  ( 0.000000000000000000, 1.000000000000000000, 0.000000000000000000 ) ) ;
#367 = DIRECTION ( 'NONE',  ( 0.000000000000000000, 1.000000000000000000, 0.000000000000000000 ) ) ;
#368 = CARTESIAN_POINT ( 'NONE',  ( 1.541131807373560481, 1.853425921617674055, -0.1039999999999998703 ) ) ;
#369 = PERSON_AND_ORGANIZATION_ROLE ( 'creator' ) ;
#370 = ORIENTED_EDGE ( 'NONE', *, *, #4389, .F. ) ;
#371 = DIRECTION ( 'NONE',  ( 0.7879377495398135478, 0.6157549048526808066, -8.018138685402973822E-15 ) ) ;
#372 = DIRECTION ( 'NONE',  ( -0.000000000000000000, -0.000000000000000000, -1.000000000000000000 ) ) ;
#373 = EDGE_CURVE ( 'NONE', #1649, #2552, #3741, .T. ) ;
#374 = EDGE_CURVE ( 'NONE', #4623, #2262, #3871, .T. ) ;
#375 = VERTEX_POINT ( 'NONE', #759 ) ;
#376 = EDGE_CURVE ( 'NONE', #6326, #5482, #5761, .T. ) ;
#377 = ORIENTED_EDGE ( 'NONE', *, *, #5359, .T. ) ;
#378 = EDGE_CURVE ( 'NONE', #845, #1086, #7789, .T. ) ;
#379 = ORIENTED_EDGE ( 'NONE', *, *, #1680, .T. ) ;
#380 = CARTESIAN_POINT ( 'NONE',  ( 1.862448717126987230, 1.453454210458644313, -0.02693779816119638154 ) ) ;
#381 = CARTESIAN_POINT ( 'NONE',  ( -0.04782642554762442377, -0.07812500000000000000, 0.07449999999999999678 ) ) ;
#382 = EDGE_CURVE ( 'NONE', #5139, #1428, #6660, .T. ) ;
#383 = DATE_AND_TIME ( #4118, #5029 ) ;
#384 = CYLINDRICAL_SURFACE ( 'NONE', #1117, 0.1799999999999999933 ) ;
#385 = EDGE_LOOP ( 'NONE', ( #2646, #2923, #1441, #6335 ) ) ;
#386 =( REPRESENTATION_RELATIONSHIP ('NONE','NONE', #3360, #5024 ) REPRESENTATION_RELATIONSHIP_WITH_TRANSFORMATION ( #2420 )SHAPE_REPRESENTATION_RELATIONSHIP( ) );
#387 = ORIENTED_EDGE ( 'NONE', *, *, #7591, .F. ) ;
#388 = ORIENTED_EDGE ( 'NONE', *, *, #6945, .T. ) ;
#389 = DIRECTION ( 'NONE',  ( -1.224646799147353207E-16, 1.000000000000000000, 0.000000000000000000 ) ) ;
#390 = UNCERTAINTY_MEASURE_WITH_UNIT (LENGTH_MEASURE( 1.000000000000000082E-05 ), #5132, 'distance_accuracy_value', 'NONE');
#391 = CARTESIAN_POINT ( 'NONE',  ( 0.1000000000000000472, -0.03125000000000000000, 0.8125000000000000000 ) ) ;
#392 = DIRECTION ( 'NONE',  ( 0.9602545086670756236, -0.2791259188691606608, 0.000000000000000000 ) ) ;
#393 = LINE ( 'NONE', #1746, #455 ) ;
#394 = CARTESIAN_POINT ( 'NONE',  ( 0.000000000000000000, 1.081250000000000044, -0.2112499999999999933 ) ) ;
#395 = FACE_OUTER_BOUND ( 'NONE', #5929, .T. ) ;
#396 = CARTESIAN_POINT ( 'NONE',  ( 1.240314151020238898, 1.658956310969642578, 0.2499999999999998890 ) ) ;
#397 = LINE ( 'NONE', #5407, #5717 ) ;
#398 = PLANE ( 'NONE',  #7750 ) ;
#399 = ORIENTED_EDGE ( 'NONE', *, *, #277, .F. ) ;
#400 = CARTESIAN_POINT ( 'NONE',  ( -0.1249999999999999445, -0.03125000000000000000, 0.06250000000000000000 ) ) ;
#401 = CARTESIAN_POINT ( 'NONE',  ( 3.672798492683009286, -8.252032378159654513, -0.1849999999999999978 ) ) ;
#402 = DIRECTION ( 'NONE',  ( 1.000000000000000000, 0.000000000000000000, 0.000000000000000000 ) ) ;
#403 = APPROVAL_ROLE ( '' ) ;
#404 = ORIENTED_EDGE ( 'NONE', *, *, #6693, .F. ) ;
#405 = FACE_OUTER_BOUND ( 'NONE', #626, .T. ) ;
#406 = CARTESIAN_POINT ( 'NONE',  ( 6.000000000000001776, 0.000000000000000000, -0.1849999999999999978 ) ) ;
#407 = DIRECTION ( 'NONE',  ( -0.000000000000000000, -0.000000000000000000, -1.000000000000000000 ) ) ;
#408 = EDGE_LOOP ( 'NONE', ( #911, #4021, #6469, #4113 ) ) ;
#409 = VERTEX_POINT ( 'NONE', #2851 ) ;
#410 = CIRCLE ( 'NONE', #5003, 0.1150000000000000050 ) ;
#411 = EDGE_CURVE ( 'NONE', #4769, #5004, #1009, .T. ) ;
#412 = EDGE_CURVE ( 'NONE', #6844, #6487, #6504, .T. ) ;
#413 = ORIENTED_EDGE ( 'NONE', *, *, #7085, .T. ) ;
#414 = ADVANCED_FACE ( 'NONE', ( #2265 ), #2758, .T. ) ;
#415 = DIRECTION ( 'NONE',  ( -0.000000000000000000, -0.000000000000000000, -1.000000000000000000 ) ) ;
#416 = AXIS2_PLACEMENT_3D ( 'NONE', #2715, #7190, #7221 ) ;
#417 = CARTESIAN_POINT ( 'NONE',  ( -1.048931738329093699, -0.7261823758192115230, 0.000000000000000000 ) ) ;
#418 = SECURITY_CLASSIFICATION ( '', '', #4964 ) ;
#419 = APPROVAL_DATE_TIME ( #4001, #6687 ) ;
#420 = DIRECTION ( 'NONE',  ( 0.7879377495398137699, 0.6157549048526804736, 0.000000000000000000 ) ) ;
#422 = EDGE_LOOP ( 'NONE', ( #1983, #4838 ) ) ;
#421 = EDGE_CURVE ( 'NONE', #5293, #7642, #2198, .T. ) ;
#423 = AXIS2_PLACEMENT_3D ( 'NONE', #5538, #4231, #4352 ) ;
#424 = APPROVAL ( #6568, 'UNSPECIFIED' ) ;
#425 = APPROVAL_PERSON_ORGANIZATION ( #1205, #7495, #5641 ) ;
#426 = EDGE_CURVE ( 'NONE', #7900, #6943, #4658, .T. ) ;
#427 = DIRECTION ( 'NONE',  ( 0.000000000000000000, 0.000000000000000000, -1.000000000000000000 ) ) ;
#428 = EDGE_CURVE ( 'NONE', #7825, #3041, #3475, .T. ) ;
#429 = VECTOR ( 'NONE', #6610, 39.37007874015748143 ) ;
#430 = DIRECTION ( 'NONE',  ( 0.000000000000000000, 0.000000000000000000, -1.000000000000000000 ) ) ;
#431 = MECHANICAL_CONTEXT ( 'NONE', #5574, 'mechanical' ) ;
#432 = DIRECTION ( 'NONE',  ( -0.000000000000000000, -0.000000000000000000, -1.000000000000000000 ) ) ;
#433 = DIRECTION ( 'NONE',  ( -0.000000000000000000, -0.000000000000000000, -1.000000000000000000 ) ) ;
#434 = ORIENTED_EDGE ( 'NONE', *, *, #2573, .T. ) ;
#435 = CARTESIAN_POINT ( 'NONE',  ( 1.472401076176925283, 1.200024862702049333, 0.2327880490291289461 ) ) ;
#436 = CARTESIAN_POINT ( 'NONE',  ( -0.09999999999999997780, 0.03125000000000000000, 0.06250000000000000000 ) ) ;
#437 = ADVANCED_FACE ( 'NONE', ( #6619 ), #5926, .T. ) ;
#438 = EDGE_CURVE ( 'NONE', #2111, #3346, #3289, .T. ) ;
#439 = AXIS2_PLACEMENT_3D ( 'NONE', #1148, #5619, #7534 ) ;
#440 = DIRECTION ( 'NONE',  ( -1.000000000000000000, 0.000000000000000000, 0.000000000000000000 ) ) ;
#441 = DIRECTION ( 'NONE',  ( 1.000000000000000000, 0.000000000000000000, 0.000000000000000000 ) ) ;
#442 = AXIS2_PLACEMENT_3D ( 'NONE', #5974, #2929, #3590 ) ;
#443 = AXIS2_PLACEMENT_3D ( 'NONE', #6754, #1707, #2984 ) ;
#444 = CARTESIAN_POINT ( 'NONE',  ( -0.09999999999999997780, -0.03125000000000000000, 0.8125000000000000000 ) ) ;
#445 = VERTEX_POINT ( 'NONE', #6042 ) ;
#446 = ORIENTED_EDGE ( 'NONE', *, *, #729, .T. ) ;
#447 = CARTESIAN_POINT ( 'NONE',  ( 2.013013176098461537E-17, 0.000000000000000000, 0.1487499999999999933 ) ) ;
#448 = SECURITY_CLASSIFICATION ( '', '', #7271 ) ;
#449 = CIRCLE ( 'NONE', #1497, 0.06199999999999999956 ) ;
#450 = CARTESIAN_POINT ( 'NONE',  ( -1.199607936389694096, -0.2200647844395000330, 0.003922330581862806982 ) ) ;
#451 = APPROVAL_DATE_TIME ( #2998, #6496 ) ;
#452 = EDGE_LOOP ( 'NONE', ( #3653, #4047, #3195, #3348, #4965, #4902, #4700, #4010 ) ) ;
#453 = DIRECTION ( 'NONE',  ( 0.000000000000000000, 0.000000000000000000, -1.000000000000000000 ) ) ;
#454 = CARTESIAN_POINT ( 'NONE',  ( 1.466665248995881576, 0.6909135088951512405, -0.1250000000000000000 ) ) ;
#455 = VECTOR ( 'NONE', #5478, 39.37007874015748143 ) ;
#456 = CIRCLE ( 'NONE', #5039, 8.513908398499122399 ) ;
#457 = PLANE ( 'NONE',  #1081 ) ;
#458 = ORIENTED_EDGE ( 'NONE', *, *, #3788, .T. ) ;
#459 = ORIENTED_EDGE ( 'NONE', *, *, #5093, .F. ) ;
#460 = AXIS2_PLACEMENT_3D ( 'NONE', #1047, #3541, #2921 ) ;
#461 = CIRCLE ( 'NONE', #3865, 0.03200000000000001454 ) ;
#462 = ORIENTED_EDGE ( 'NONE', *, *, #7249, .T. ) ;
#463 = DIRECTION ( 'NONE',  ( -1.000000000000000000, 0.000000000000000000, 0.000000000000000000 ) ) ;
#464 = CARTESIAN_POINT ( 'NONE',  ( 0.09776754390993486199, -0.4589828842714404611, 0.2234246117937112586 ) ) ;
#465 = DIRECTION ( 'NONE',  ( 1.000000000000000000, -1.713662733658207664E-13, 0.000000000000000000 ) ) ;
#466 = EDGE_LOOP ( 'NONE', ( #6355, #1368, #7116, #5850 ) ) ;
#467 = VECTOR ( 'NONE', #1230, 39.37007874015748143 ) ;
#468 = ORIENTED_EDGE ( 'NONE', *, *, #523, .T. ) ;
#469 = EDGE_CURVE ( 'NONE', #1621, #2575, #7157, .T. ) ;
#470 = DIRECTION ( 'NONE',  ( 1.000000000000000000, 0.000000000000000000, 0.000000000000000000 ) ) ;
#471 = AXIS2_PLACEMENT_3D ( 'NONE', #5489, #2945, #5524 ) ;
#472 = CARTESIAN_POINT ( 'NONE',  ( -1.411633252941551619, 0.8434166392007494961, 0.09374999999999998612 ) ) ;
#473 = DIRECTION ( 'NONE',  ( -0.2853335501257686646, 0.9584282785752022971, 0.000000000000000000 ) ) ;
#474 = CALENDAR_DATE ( 2026, 9, 10 ) ;
#475 = DIRECTION ( 'NONE',  ( 0.000000000000000000, 0.000000000000000000, -1.000000000000000000 ) ) ;
#476 = DIRECTION ( 'NONE',  ( 0.000000000000000000, -1.000000000000000000, 0.000000000000000000 ) ) ;
#477 = VERTEX_POINT ( 'NONE', #4119 ) ;
#478 = CIRCLE ( 'NONE', #3624, 6.930657474112426719 ) ;
#479 = AXIS2_PLACEMENT_3D ( 'NONE', #2095, #6484, #870 ) ;
#480 = CARTESIAN_POINT ( 'NONE',  ( 1.569663840435087332, 1.236826606985905519, 0.1968643041809139405 ) ) ;
#481 = CARTESIAN_POINT ( 'NONE',  ( -4.882388066182508091, 5.670153330992292240, 0.03199999999999999373 ) ) ;
#482 = EDGE_CURVE ( 'NONE', #5571, #5067, #6879, .T. ) ;
#483 = ADVANCED_FACE ( 'NONE', ( #7869 ), #3390, .T. ) ;
#484 = CIRCLE ( 'NONE', #7425, 0.1250000000000000000 ) ;
#485 = CIRCLE ( 'NONE', #8063, 0.5000000000000279776 ) ;
#486 = CC_DESIGN_DATE_AND_TIME_ASSIGNMENT ( #5507, #1123, ( #1357 ) ) ;
#487 = DIRECTION ( 'NONE',  ( -0.6157549048526803626, 0.7879377495398141029, -0.000000000000000000 ) ) ;
#488 = ADVANCED_FACE ( 'NONE', ( #5318 ), #8044, .T. ) ;
#489 = CARTESIAN_POINT ( 'NONE',  ( -0.1250000000000000000, 0.6250000000000000000, 0.03125000000000000000 ) ) ;
#490 = EDGE_LOOP ( 'NONE', ( #1027, #4132, #2110, #7205 ) ) ;
#491 = VECTOR ( 'NONE', #6268, 39.37007874015748143 ) ;
#492 = DIRECTION ( 'NONE',  ( -0.000000000000000000, -1.000000000000000000, -0.000000000000000000 ) ) ;
#493 = AXIS2_PLACEMENT_3D ( 'NONE', #3613, #5577, #1716 ) ;
#494 = DIRECTION ( 'NONE',  ( 0.000000000000000000, 0.000000000000000000, 1.000000000000000000 ) ) ;
#495 = CYLINDRICAL_SURFACE ( 'NONE', #3375, 0.1250000000000000000 ) ;
#496 = MECHANICAL_CONTEXT ( 'NONE', #2361, 'mechanical' ) ;
#497 = ORIENTED_EDGE ( 'NONE', *, *, #4721, .F. ) ;
#498 = CARTESIAN_POINT ( 'NONE',  ( 1.846835003037430534, 1.498370261438588313, 0.2500000000000000000 ) ) ;
#499 = CARTESIAN_POINT ( 'NONE',  ( 1.082008577329383270, 0.9412886604515813271, 0.000000000000000000 ) ) ;
#500 = CARTESIAN_POINT ( 'NONE',  ( 1.584026930697933766, 1.313829542709616272, 0.2488199491279635966 ) ) ;
#501 = ORIENTED_EDGE ( 'NONE', *, *, #4788, .T. ) ;
#502 = VERTEX_POINT ( 'NONE', #7802 ) ;
#503 = CARTESIAN_POINT ( 'NONE',  ( 1.258671604940865274, -0.02501003737716508274, -0.1849999999999999978 ) ) ;
#504 =( NAMED_UNIT ( * ) PLANE_ANGLE_UNIT ( ) SI_UNIT ( $, .RADIAN. ) );
#505 = ORIENTED_EDGE ( 'NONE', *, *, #4721, .T. ) ;
#506 = DIRECTION ( 'NONE',  ( -0.7879377495398141029, -0.6157549048526801405, -7.102804783527083974E-15 ) ) ;
#507 = APPROVAL_DATE_TIME ( #4200, #1233 ) ;
#508 = CARTESIAN_POINT ( 'NONE',  ( 1.501632106627864172, 1.101688700216157502, 0.2499999999999998335 ) ) ;
#509 = CARTESIAN_POINT ( 'NONE',  ( 6.190219624525621356, 0.4584813330253886265, -0.1250000000000000000 ) ) ;
#510 = FACE_OUTER_BOUND ( 'NONE', #4661, .T. ) ;
#511 = DIRECTION ( 'NONE',  ( -1.000000000000000000, 0.000000000000000000, 0.000000000000000000 ) ) ;
#512 = APPLICATION_PROTOCOL_DEFINITION ( 'international standard', 'config_control_design', 1994, #4207 ) ;
#513 = CARTESIAN_POINT ( 'NONE',  ( 0.000000000000000000, 1.362500000000000044, 0.1250000000000000000 ) ) ;
#514 = DIRECTION ( 'NONE',  ( 0.000000000000000000, -1.000000000000000000, 0.000000000000000000 ) ) ;
#515 = ORIENTED_EDGE ( 'NONE', *, *, #7744, .T. ) ;
#516 = CARTESIAN_POINT ( 'NONE',  ( 1.533263802984024204, 1.243817105212362328, 0.2362054852279182326 ) ) ;
#517 = CARTESIAN_POINT ( 'NONE',  ( 0.1743677072153199392, -0.4209564106690024676, 0.1250000000000000000 ) ) ;
#518 = VERTEX_POINT ( 'NONE', #1574 ) ;
#519 = CARTESIAN_POINT ( 'NONE',  ( 1.258616367985684104, -0.02482036785324303815, 0.1250000000000000000 ) ) ;
#520 = CARTESIAN_POINT ( 'NONE',  ( 1.299553592491851761, 1.066832042848483653, -0.05797701948372137315 ) ) ;
#521 = ADVANCED_FACE ( 'NONE', ( #6580 ), #384, .T. ) ;
#522 = EDGE_CURVE ( 'NONE', #3956, #2990, #4520, .T. ) ;
#523 = EDGE_CURVE ( 'NONE', #4775, #2638, #5633, .T. ) ;
#524 = PERSON ( 'NAUO-PER2', 'UNSPECIFIED', 'UNSPECIFIED', ('UNSPECIFIED'), ('UNSPECIFIED'), ('UNSPECIFIED') ) ;
#525 = FACE_OUTER_BOUND ( 'NONE', #948, .T. ) ;
#526 = VERTEX_POINT ( 'NONE', #3046 ) ;
#527 = CARTESIAN_POINT ( 'NONE',  ( 0.03125000000000000000, 0.000000000000000000, -0.1162848326531996102 ) ) ;
#528 = EDGE_CURVE ( 'NONE', #2262, #7983, #5913, .T. ) ;
#529 = DIRECTION ( 'NONE',  ( 0.6157549048561230531, -0.7879377495371234774, 0.000000000000000000 ) ) ;
#530 = DIRECTION ( 'NONE',  ( 0.9602545086670756236, -0.2791259188691606608, 0.000000000000000000 ) ) ;
#531 = PERSON_AND_ORGANIZATION_ROLE ( 'classification_officer' ) ;
#532 = EDGE_LOOP ( 'NONE', ( #5100, #4338, #7008, #118, #2763, #4689, #2797, #216 ) ) ;
#533 = CARTESIAN_POINT ( 'NONE',  ( -0.1054677083281892608, 0.5625000000000000000, 0.03125000000000000000 ) ) ;
#534 = CARTESIAN_POINT ( 'NONE',  ( 0.2896281645421511231, -0.04777128394798136474, 0.07449999999999999678 ) ) ;
#535 = ORIENTED_EDGE ( 'NONE', *, *, #2466, .T. ) ;
#536 = CARTESIAN_POINT ( 'NONE',  ( 1.669934150624661440, 1.364734201194776286, 0.2262543876504554130 ) ) ;
#537 = ORIENTED_EDGE ( 'NONE', *, *, #411, .T. ) ;
#538 = DIRECTION ( 'NONE',  ( 0.7879377495398138809, 0.6157549048526802515, 0.000000000000000000 ) ) ;
#539 = DIRECTION ( 'NONE',  ( 0.000000000000000000, 1.000000000000000000, 0.000000000000000000 ) ) ;
#540 = PERSON_AND_ORGANIZATION ( #2875, #7647 ) ;
#541 = CARTESIAN_POINT ( 'NONE',  ( 1.723350842796532278, 1.129006085766179890, -0.1039999999999998703 ) ) ;
#542 = CC_DESIGN_SECURITY_CLASSIFICATION ( #6696, ( #8092 ) ) ;
#543 = LOCAL_TIME ( 14, 45, 32.00000000000000000, #6138 ) ;
#544 = CARTESIAN_POINT ( 'NONE',  ( 0.000000000000000000, 0.6124999999999999334, 0.03125000000000000000 ) ) ;
#545 = DIRECTION ( 'NONE',  ( 1.000000000000000000, 1.942647462161253450E-15, 0.000000000000000000 ) ) ;
#546 = PLANE ( 'NONE',  #710 ) ;
#547 = PERSON_AND_ORGANIZATION ( #4735, #6190 ) ;
#548 = DIRECTION ( 'NONE',  ( -0.000000000000000000, -0.000000000000000000, -1.000000000000000000 ) ) ;
#549 = FACE_OUTER_BOUND ( 'NONE', #7220, .T. ) ;
#550 = AXIS2_PLACEMENT_3D ( 'NONE', #1792, #4787, #4743 ) ;
#551 = ORIENTED_EDGE ( 'NONE', *, *, #3385, .F. ) ;
#552 = CARTESIAN_POINT ( 'NONE',  ( 1.602182050848640182, 1.261380129295977648, 0.2011192772941635953 ) ) ;
#553 =( GEOMETRIC_REPRESENTATION_CONTEXT ( 3 ) GLOBAL_UNCERTAINTY_ASSIGNED_CONTEXT ( ( #1860 ) ) GLOBAL_UNIT_ASSIGNED_CONTEXT ( ( #3627, #504, #3086 ) ) REPRESENTATION_CONTEXT ( 'NONE', 'WORKASPACE' ) );
#554 = TOROIDAL_SURFACE ( 'NONE', #4882, 0.1255000000000000282, 0.06199999999999999956 ) ;
#555 = ORIENTED_EDGE ( 'NONE', *, *, #884, .F. ) ;
#556 = DIRECTION ( 'NONE',  ( -0.2791259188691606608, -0.9602545086670756236, -0.000000000000000000 ) ) ;
#557 = PLANE ( 'NONE',  #1790 ) ;
#558 = LINE ( 'NONE', #2358, #607 ) ;
#559 = ORIENTED_EDGE ( 'NONE', *, *, #5593, .F. ) ;
#560 = VECTOR ( 'NONE', #1957, 39.37007874015748143 ) ;
#561 = CARTESIAN_POINT ( 'NONE',  ( 0.000000000000000000, 0.000000000000000000, 0.06300000000000000044 ) ) ;
#562 = EDGE_CURVE ( 'NONE', #5236, #762, #5047, .T. ) ;
#563 = ADVANCED_FACE ( 'NONE', ( #10 ), #723, .T. ) ;
#564 = AXIS2_PLACEMENT_3D ( 'NONE', #1487, #6500, #5267 ) ;
#565 = CARTESIAN_POINT ( 'NONE',  ( 6.191327929239395012, 0.4578608198540752294, 0.1850000000000003586 ) ) ;
#566 = CARTESIAN_POINT ( 'NONE',  ( 1.347111479062088626E-17, 0.000000000000000000, -0.1100000000000000006 ) ) ;
#567 = CALENDAR_DATE ( 2026, 9, 10 ) ;
#568 = ORIENTED_EDGE ( 'NONE', *, *, #1673, .F. ) ;
#569 = CARTESIAN_POINT ( 'NONE',  ( 2.023273750469992349E-18, 0.03125000000000000000, 0.3061494484901324808 ) ) ;
#570 = DIRECTION ( 'NONE',  ( -0.000000000000000000, -0.000000000000000000, 1.000000000000000000 ) ) ;
#571 = ORIENTED_EDGE ( 'NONE', *, *, #1578, .T. ) ;
#572 = FACE_OUTER_BOUND ( 'NONE', #1266, .T. ) ;
#573 = EDGE_CURVE ( 'NONE', #1449, #3669, #5575, .T. ) ;
#574 = CIRCLE ( 'NONE', #5153, 0.4060000000000001386 ) ;
#575 = AXIS2_PLACEMENT_3D ( 'NONE', #6975, #1395, #4409 ) ;
#576 = EDGE_CURVE ( 'NONE', #2354, #2564, #63, .T. ) ;
#577 = VERTEX_POINT ( 'NONE', #5471 ) ;
#578 = EDGE_CURVE ( 'NONE', #7112, #6856, #2382, .T. ) ;
#579 = CARTESIAN_POINT ( 'NONE',  ( 1.848231205201100513, 1.461457015412791716, 0.03105351328329579094 ) ) ;
#580 = ORGANIZATION ( 'NAUO-ORG4', 'UNSPECIFIED', 'UNSPECIFIED' ) ;
#581 = CARTESIAN_POINT ( 'NONE',  ( 6.067386035484801710, 0.2407470087491039856, 0.1250000000000000000 ) ) ;
#582 = AXIS2_PLACEMENT_3D ( 'NONE', #2056, #3937, #331 ) ;
#583 = APPROVAL_STATUS ( 'not_yet_approved' ) ;
#584 = CC_DESIGN_PERSON_AND_ORGANIZATION_ASSIGNMENT ( #4466, #1305, ( #7867 ) ) ;
#585 = FACE_OUTER_BOUND ( 'NONE', #4092, .T. ) ;
#586 = ADVANCED_FACE ( 'NONE', ( #585 ), #7958, .T. ) ;
#587 = CIRCLE ( 'NONE', #3993, 0.1250000000000000000 ) ;
#588 = AXIS2_PLACEMENT_3D ( 'NONE', #2364, #6723, #1107 ) ;
#589 = ORIENTED_EDGE ( 'NONE', *, *, #2671, .T. ) ;
#590 = DIRECTION ( 'NONE',  ( -0.000000000000000000, -1.000000000000000000, -0.000000000000000000 ) ) ;
#591 = DIRECTION ( 'NONE',  ( 0.6568496200222108117, 0.7540216022612863389, -0.000000000000000000 ) ) ;
#592 = CARTESIAN_POINT ( 'NONE',  ( 0.009791616623485311505, -0.4636505048871231160, 0.003820833004121301866 ) ) ;
#593 = DATE_AND_TIME ( #4253, #5126 ) ;
#594 = DIRECTION ( 'NONE',  ( 0.000000000000000000, 1.000000000000000000, 0.000000000000000000 ) ) ;
#595 = CARTESIAN_POINT ( 'NONE',  ( 1.842690855593505317, 1.503127479225555785, 6.120881109992683290E-14 ) ) ;
#596 = VECTOR ( 'NONE', #1736, 39.37007874015748143 ) ;
#597 = ORIENTED_EDGE ( 'NONE', *, *, #6829, .T. ) ;
#598 = EDGE_CURVE ( 'NONE', #1607, #1086, #1853, .T. ) ;
#599 = FACE_OUTER_BOUND ( 'NONE', #452, .T. ) ;
#600 = VECTOR ( 'NONE', #1687, 39.37007874015748143 ) ;
#601 = ORIENTED_EDGE ( 'NONE', *, *, #1330, .T. ) ;
#603 = DIRECTION ( 'NONE',  ( -1.000000000000000000, 0.000000000000000000, 0.000000000000000000 ) ) ;
#602 = CIRCLE ( 'NONE', #6366, 0.1250000000000000000 ) ;
#604 = DIRECTION ( 'NONE',  ( -0.9726399823210830631, -0.2323175946639496336, 0.000000000000000000 ) ) ;
#605 = CIRCLE ( 'NONE', #3230, 0.2499400561648078278 ) ;
#606 = CARTESIAN_POINT ( 'NONE',  ( 1.723083782080649939, 1.395997476760423961, 0.1965221205739769994 ) ) ;
#607 = VECTOR ( 'NONE', #3065, 39.37007874015748143 ) ;
#608 = EDGE_LOOP ( 'NONE', ( #844, #5618, #7567, #2480 ) ) ;
#609 = CARTESIAN_POINT ( 'NONE',  ( 1.600980465589876944, 1.204709832745134657, 0.1951356537883363329 ) ) ;
#610 = EDGE_LOOP ( 'NONE', ( #3449, #8076, #1071, #6987 ) ) ;
#611 = AXIS2_PLACEMENT_3D ( 'NONE', #5435, #475, #6139 ) ;
#612 = CIRCLE ( 'NONE', #479, 0.1487499999999999933 ) ;
#613 = ORIENTED_EDGE ( 'NONE', *, *, #7841, .F. ) ;
#614 = CARTESIAN_POINT ( 'NONE',  ( 6.190221022838899856, 0.4584861219976859026, -0.1250000000000004441 ) ) ;
#615 = CARTESIAN_POINT ( 'NONE',  ( 3.690413561029368683, -8.374393170229348371, 0.1250000000000000000 ) ) ;
#616 = PERSON_AND_ORGANIZATION ( #4735, #6190 ) ;
#617 = ORIENTED_EDGE ( 'NONE', *, *, #5992, .F. ) ;
#618 = CARTESIAN_POINT ( 'NONE',  ( 0.000000000000000000, 0.6350000000000000089, 0.000000000000000000 ) ) ;
#619 = CIRCLE ( 'NONE', #7940, 0.06200000000000004813 ) ;
#620 = FACE_OUTER_BOUND ( 'NONE', #6980, .T. ) ;
#621 = ADVANCED_FACE ( 'NONE', ( #4239 ), #8034, .T. ) ;
#622 = ADVANCED_FACE ( 'NONE', ( #4895 ), #6816, .T. ) ;
#623 = ORIENTED_EDGE ( 'NONE', *, *, #5945, .T. ) ;
#624 = CARTESIAN_POINT ( 'NONE',  ( -0.03125000000000000000, 0.03124999999999997571, -0.1106726592253027830 ) ) ;
#625 = AXIS2_PLACEMENT_3D ( 'NONE', #5114, #5818, #5706 ) ;
#626 = EDGE_LOOP ( 'NONE', ( #4, #893, #3243, #6088, #4823 ) ) ;
#627 = AXIS2_PLACEMENT_3D ( 'NONE', #3489, #7212, #920 ) ;
#628 = DIRECTION ( 'NONE',  ( -0.8680936205257682170, 0.4964005096718413501, 0.000000000000000000 ) ) ;
#629 = COORDINATED_UNIVERSAL_TIME_OFFSET ( 0, 0, .AHEAD. ) ;
#630 = FACE_OUTER_BOUND ( 'NONE', #3426, .T. ) ;
#631 = DATE_AND_TIME ( #1735, #3986 ) ;
#632 = CARTESIAN_POINT ( 'NONE',  ( 1.356840083662244734, 0.003162463486408387866, 0.000000000000000000 ) ) ;
#633 = ADVANCED_FACE ( 'NONE', ( #3581 ), #5594, .F. ) ;
#634 = EDGE_CURVE ( 'NONE', #6740, #6273, #7661, .T. ) ;
#635 = ADVANCED_FACE ( 'NONE', ( #8075 ), #6236, .F. ) ;
#636 = EDGE_CURVE ( 'NONE', #140, #3222, #3668, .T. ) ;
#637 = ORIENTED_EDGE ( 'NONE', *, *, #6793, .F. ) ;
#638 = CARTESIAN_POINT ( 'NONE',  ( 1.150973126671910540, 0.8530396325060728424, -0.3750000000000000555 ) ) ;
#639 = CARTESIAN_POINT ( 'NONE',  ( -0.9280291358773672394, 0.8548654847802351631, 0.1250000000000000000 ) ) ;
#640 = DIRECTION ( 'NONE',  ( -0.000000000000000000, -0.000000000000000000, -1.000000000000000000 ) ) ;
#641 = PERSON_AND_ORGANIZATION ( #4735, #6190 ) ;
#642 = DIRECTION ( 'NONE',  ( -0.8875604078987033851, 0.4606913525677331367, 0.000000000000000000 ) ) ;
#643 = DIRECTION ( 'NONE',  ( 0.000000000000000000, 0.000000000000000000, 1.000000000000000000 ) ) ;
#644 = ORIENTED_EDGE ( 'NONE', *, *, #2466, .F. ) ;
#645 = ORIENTED_EDGE ( 'NONE', *, *, #7249, .F. ) ;
#646 = VERTEX_POINT ( 'NONE', #4410 ) ;
#647 = ORIENTED_EDGE ( 'NONE', *, *, #2335, .T. ) ;
#648 = CYLINDRICAL_SURFACE ( 'NONE', #313, 0.4060000000000001386 ) ;
#649 = CARTESIAN_POINT ( 'NONE',  ( -1.543211452806561912, 0.6927940070358482583, 0.1250000000000000000 ) ) ;
#650 = DIRECTION ( 'NONE',  ( -0.6157549048526823610, 0.7879377495398123266, 0.000000000000000000 ) ) ;
#651 = EDGE_LOOP ( 'NONE', ( #2721, #1905, #2051, #7914, #1897, #7051, #4383, #3537 ) ) ;
#652 = CARTESIAN_POINT ( 'NONE',  ( 2.387087291339119677, -6.013863021948615106, 0.1250000000000000000 ) ) ;
#653 = EDGE_LOOP ( 'NONE', ( #3292, #4215, #3792, #3302 ) ) ;
#654 = DIMENSIONAL_EXPONENTS ( 1.000000000000000000, 0.000000000000000000, 0.000000000000000000, 0.000000000000000000, 0.000000000000000000, 0.000000000000000000, 0.000000000000000000 ) ;
#655 = FACE_OUTER_BOUND ( 'NONE', #7525, .T. ) ;
#656 = DIRECTION ( 'NONE',  ( 0.8680936205257663296, -0.4964005096718442922, 0.000000000000000000 ) ) ;
#657 = DATE_TIME_ROLE ( 'classification_date' ) ;
#658 = VERTEX_POINT ( 'NONE', #667 ) ;
#659 = DIRECTION ( 'NONE',  ( -0.7879377495398141029, -0.6157549048526800295, 0.000000000000000000 ) ) ;
#660 = DIRECTION ( 'NONE',  ( -0.000000000000000000, -0.000000000000000000, -1.000000000000000000 ) ) ;
#661 = VERTEX_POINT ( 'NONE', #5057 ) ;
#662 = DIRECTION ( 'NONE',  ( -0.6568496200222107007, -0.7540216022612863389, 0.000000000000000000 ) ) ;
#663 = DIRECTION ( 'NONE',  ( -1.821231995776175725E-16, -1.000000000000000000, 0.000000000000000000 ) ) ;
#664 = DIRECTION ( 'NONE',  ( 8.441663814850090885E-16, 1.362795760884335312E-15, -1.000000000000000000 ) ) ;
#665 = DIRECTION ( 'NONE',  ( 0.000000000000000000, 0.000000000000000000, 1.000000000000000000 ) ) ;
#666 = APPROVAL_STATUS ( 'not_yet_approved' ) ;
#667 = CARTESIAN_POINT ( 'NONE',  ( -1.763630694164995738, 1.150051601412733771, -0.3269762307749164432 ) ) ;
#668 = VERTEX_POINT ( 'NONE', #709 ) ;
#669 = EDGE_CURVE ( 'NONE', #1476, #3995, #4406, .T. ) ;
#670 = EDGE_CURVE ( 'NONE', #4959, #297, #4919, .T. ) ;
#671 = CARTESIAN_POINT ( 'NONE',  ( -1.067641779222573639, 0.6107141540073635078, 0.1250000000000000000 ) ) ;
#672 = DIRECTION ( 'NONE',  ( -1.000000000000000000, -8.862153517038291156E-15, 0.000000000000000000 ) ) ;
#673 = CARTESIAN_POINT ( 'NONE',  ( 0.09770155834983287879, -0.4589921552484208522, 0.02653900339155101928 ) ) ;
#674 = PERSON_AND_ORGANIZATION_ROLE ( 'creator' ) ;
#675 = DIRECTION ( 'NONE',  ( 1.000000000000000000, 0.000000000000000000, 0.000000000000000000 ) ) ;
#676 = LINE ( 'NONE', #2631, #5037 ) ;
#677 = EDGE_LOOP ( 'NONE', ( #6726, #2915, #5765, #4975, #2876, #3002, #3508 ) ) ;
#678 = CC_DESIGN_DATE_AND_TIME_ASSIGNMENT ( #251, #334, ( #6001 ) ) ;
#679 = EDGE_CURVE ( 'NONE', #4615, #6638, #5834, .T. ) ;
#680 = CIRCLE ( 'NONE', #1199, 0.1250000000000000000 ) ;
#681 = LOCAL_TIME ( 14, 45, 32.00000000000000000, #698 ) ;
#682 = ADVANCED_FACE ( 'NONE', ( #1313 ), #2061, .T. ) ;
#683 = CARTESIAN_POINT ( 'NONE',  ( 0.9887166869077879117, 0.8277708867933823988, 0.2179999999999999993 ) ) ;
#684 = VERTEX_POINT ( 'NONE', #2618 ) ;
#685 = AXIS2_PLACEMENT_3D ( 'NONE', #394, #3596, #4129 ) ;
#686 = DIRECTION ( 'NONE',  ( 0.7540216022612858948, -0.6568496200222110337, 0.000000000000000000 ) ) ;
#687 = DIRECTION ( 'NONE',  ( 0.000000000000000000, 0.000000000000000000, 1.000000000000000000 ) ) ;
#688 = CC_DESIGN_APPROVAL ( #4742, ( #5666 ) ) ;
#689 = CC_DESIGN_PERSON_AND_ORGANIZATION_ASSIGNMENT ( #6476, #3314, ( #5523 ) ) ;
#690 = DIRECTION ( 'NONE',  ( 1.000000000000000000, 0.000000000000000000, 0.000000000000000000 ) ) ;
#691 = EDGE_CURVE ( 'NONE', #1756, #1913, #1003, .T. ) ;
#692 = ORIENTED_EDGE ( 'NONE', *, *, #5297, .T. ) ;
#693 = DIRECTION ( 'NONE',  ( -1.000000000000000000, 0.000000000000000000, -0.000000000000000000 ) ) ;
#694 = AXIS2_PLACEMENT_3D ( 'NONE', #1480, #3988, #2752 ) ;
#695 = VERTEX_POINT ( 'NONE', #5752 ) ;
#696 = LINE ( 'NONE', #35, #1509 ) ;
#697 = CARTESIAN_POINT ( 'NONE',  ( -0.1210307295689817680, 0.6250000000000000000, 0.03125000000000000000 ) ) ;
#698 = COORDINATED_UNIVERSAL_TIME_OFFSET ( 0, 0, .AHEAD. ) ;
#699 = ORIENTED_EDGE ( 'NONE', *, *, #6003, .F. ) ;
#700 = AXIS2_PLACEMENT_3D ( 'NONE', #652, #32, #5035 ) ;
#701 = CARTESIAN_POINT ( 'NONE',  ( 0.000000000000000000, 0.03125000000000000000, 0.6646281645421511231 ) ) ;
#702 = APPLICATION_CONTEXT ( 'configuration controlled 3d designs of mechanical parts and assemblies' ) ;
#703 = DIRECTION ( 'NONE',  ( 0.7879377495398138809, 0.6157549048526804736, 0.000000000000000000 ) ) ;
#704 = DIRECTION ( 'NONE',  ( 0.000000000000000000, -0.000000000000000000, -1.000000000000000000 ) ) ;
#705 = AXIS2_PLACEMENT_3D ( 'NONE', #4868, #7365, #4259 ) ;
#706 = DIRECTION ( 'NONE',  ( -0.000000000000000000, -0.000000000000000000, 1.000000000000000000 ) ) ;
#707 = APPLICATION_PROTOCOL_DEFINITION ( 'international standard', 'config_control_design', 1994, #1950 ) ;
#708 = DIRECTION ( 'NONE',  ( -1.000000000000000000, 0.000000000000000000, 0.000000000000000000 ) ) ;
#709 = CARTESIAN_POINT ( 'NONE',  ( 0.03125000000000000000, 0.03124999999999997571, -0.1106726592253027830 ) ) ;
#710 = AXIS2_PLACEMENT_3D ( 'NONE', #8082, #7358, #6820 ) ;
#711 = AXIS2_PLACEMENT_3D ( 'NONE', #6403, #5171, #708 ) ;
#712 = VECTOR ( 'NONE', #5279, 39.37007874015748143 ) ;
#713 = VERTEX_POINT ( 'NONE', #5673 ) ;
#714 = LINE ( 'NONE', #5722, #7514 ) ;
#715 = APPROVAL_ROLE ( '' ) ;
#716 = DIRECTION ( 'NONE',  ( -0.9726399823210832851, -0.2323175946639495226, -4.958252772465767332E-16 ) ) ;
#717 = ORIENTED_EDGE ( 'NONE', *, *, #7786, .F. ) ;
#718 = VECTOR ( 'NONE', #514, 39.37007874015748143 ) ;
#719 = EDGE_CURVE ( 'NONE', #3809, #2089, #1377, .T. ) ;
#720 = VECTOR ( 'NONE', #7897, 39.37007874015748854 ) ;
#721 = ORIENTED_EDGE ( 'NONE', *, *, #4440, .F. ) ;
#722 = DIRECTION ( 'NONE',  ( 0.000000000000000000, 0.000000000000000000, 1.000000000000000000 ) ) ;
#723 = TOROIDAL_SURFACE ( 'NONE', #1771, 0.09374999999999998612, 0.03125000000000000000 ) ;
#724 = ORIENTED_EDGE ( 'NONE', *, *, #7926, .F. ) ;
#725 = CARTESIAN_POINT ( 'NONE',  ( 1.566033889679777413, 1.280741487518077371, 0.2500000000000000555 ) ) ;
#726 = DIRECTION ( 'NONE',  ( 0.000000000000000000, 0.000000000000000000, 1.000000000000000000 ) ) ;
#727 = DIRECTION ( 'NONE',  ( -0.000000000000000000, -1.000000000000000000, -0.000000000000000000 ) ) ;
#728 = EDGE_CURVE ( 'NONE', #6037, #2029, #73, .T. ) ;
#729 = EDGE_CURVE ( 'NONE', #518, #2698, #3359, .T. ) ;
#730 = CYLINDRICAL_SURFACE ( 'NONE', #8013, 0.3243589946935200308 ) ;
#731 = VECTOR ( 'NONE', #2411, 39.37007874015748143 ) ;
#732 = EDGE_CURVE ( 'NONE', #5878, #4081, #2960, .T. ) ;
#733 = ORIENTED_EDGE ( 'NONE', *, *, #3536, .T. ) ;
#734 = CARTESIAN_POINT ( 'NONE',  ( 1.855189785566745853, 1.467426056222693953, 0.009546785084580650116 ) ) ;
#735 = DIRECTION ( 'NONE',  ( 0.6568496200222108117, 0.7540216022612861169, 0.000000000000000000 ) ) ;
#736 = AXIS2_PLACEMENT_3D ( 'NONE', #3557, #3024, #2446 ) ;
#737 = PERSON_AND_ORGANIZATION ( #4735, #6190 ) ;
#738 = ORIENTED_EDGE ( 'NONE', *, *, #7841, .T. ) ;
#739 = CARTESIAN_POINT ( 'NONE',  ( 1.251261725424357429, 1.073556033307649704, -0.06746410551919426735 ) ) ;
#740 = DIRECTION ( 'NONE',  ( 0.000000000000000000, 0.000000000000000000, -1.000000000000000000 ) ) ;
#741 = ORIENTED_EDGE ( 'NONE', *, *, #1281, .F. ) ;
#742 = AXIS2_PLACEMENT_3D ( 'NONE', #6023, #6636, #1025 ) ;
#743 = CARTESIAN_POINT ( 'NONE',  ( -1.040997396242601791, -0.7528336330030669377, 0.2179999999999999993 ) ) ;
#744 = AXIS2_PLACEMENT_3D ( 'NONE', #1815, #5544, #1898 ) ;
#745 = CIRCLE ( 'NONE', #3110, 0.2812500000000000555 ) ;
#746 = DIRECTION ( 'NONE',  ( -0.000000000000000000, -1.000000000000000000, -0.000000000000000000 ) ) ;
#747 = PERSON_AND_ORGANIZATION ( #4735, #6190 ) ;
#748 = CARTESIAN_POINT ( 'NONE',  ( -1.411633252941551619, 0.8434166392007494961, -0.09374999999999998612 ) ) ;
#749 = PERSON_AND_ORGANIZATION_ROLE ( 'classification_officer' ) ;
#750 = CARTESIAN_POINT ( 'NONE',  ( 0.000000000000000000, 0.6124999999999999334, 0.000000000000000000 ) ) ;
#751 = CARTESIAN_POINT ( 'NONE',  ( 1.735403701365888285, 1.408497115441140757, 0.2316522750339969627 ) ) ;
#752 = AXIS2_PLACEMENT_3D ( 'NONE', #6453, #5459, #2909 ) ;
#753 = AXIS2_PLACEMENT_3D ( 'NONE', #889, #7155, #2264 ) ;
#754 = EDGE_LOOP ( 'NONE', ( #1499, #5423, #1970, #4121 ) ) ;
#755 = DIRECTION ( 'NONE',  ( 0.000000000000000000, 0.000000000000000000, 1.000000000000000000 ) ) ;
#756 = CARTESIAN_POINT ( 'NONE',  ( -0.06999999999999996503, -0.03125000000000000000, 0.8125000000000000000 ) ) ;
#757 = DATE_AND_TIME ( #3830, #7620 ) ;
#758 = DIRECTION ( 'NONE',  ( 0.7540216022612862279, -0.6568496200222107007, -0.000000000000000000 ) ) ;
#759 = CARTESIAN_POINT ( 'NONE',  ( -1.763630694164994850, 1.150051601412733771, 0.1649762307749162715 ) ) ;
#760 = ORIENTED_EDGE ( 'NONE', *, *, #780, .F. ) ;
#761 = VERTEX_POINT ( 'NONE', #3250 ) ;
#762 = VERTEX_POINT ( 'NONE', #1967 ) ;
#763 = CARTESIAN_POINT ( 'NONE',  ( -1.803041671366328202, 1.104810305277057259, -0.3269762307749163877 ) ) ;
#764 = ORIENTED_EDGE ( 'NONE', *, *, #3989, .F. ) ;
#765 = CARTESIAN_POINT ( 'NONE',  ( 1.592784593561623607, 1.300866851810909886, 0.2489796966440675774 ) ) ;
#766 = DIRECTION ( 'NONE',  ( 0.000000000000000000, 0.000000000000000000, -1.000000000000000000 ) ) ;
#767 = DIRECTION ( 'NONE',  ( 0.000000000000000000, -0.000000000000000000, -1.000000000000000000 ) ) ;
#768 = DIRECTION ( 'NONE',  ( -1.000000000000000000, 0.000000000000000000, -0.000000000000000000 ) ) ;
#769 = ORIENTED_EDGE ( 'NONE', *, *, #2647, .T. ) ;
#770 = ADVANCED_FACE ( 'NONE', ( #6902 ), #4445, .T. ) ;
#771 = CARTESIAN_POINT ( 'NONE',  ( 1.849479720061930399, 1.475133735913631616, 0.03415326110672887300 ) ) ;
#772 = DIRECTION ( 'NONE',  ( 0.000000000000000000, 0.000000000000000000, 1.000000000000000000 ) ) ;
#773 = DATE_AND_TIME ( #4348, #3434 ) ;
#774 = VERTEX_POINT ( 'NONE', #3907 ) ;
#775 = PLANE ( 'NONE',  #4281 ) ;
#776 = CARTESIAN_POINT ( 'NONE',  ( -0.1875000000000000278, 2.296212748401287726E-17, -0.6219999999999999973 ) ) ;
#777 = VERTEX_POINT ( 'NONE', #824 ) ;
#778 = CARTESIAN_POINT ( 'NONE',  ( 1.552296370367317158, 1.257885440169557612, 0.2367010496530764507 ) ) ;
#779 = CC_DESIGN_PERSON_AND_ORGANIZATION_ASSIGNMENT ( #6402, #783, ( #5402 ) ) ;
#780 = EDGE_CURVE ( 'NONE', #6611, #6939, #33, .T. ) ;
#781 = EDGE_CURVE ( 'NONE', #4837, #7187, #5801, .T. ) ;
#782 = DIRECTION ( 'NONE',  ( -0.000000000000000000, -0.000000000000000000, -1.000000000000000000 ) ) ;
#783 = PERSON_AND_ORGANIZATION_ROLE ( 'creator' ) ;
#784 = CARTESIAN_POINT ( 'NONE',  ( 1.437142212823555587, 1.212327995211809117, 0.2500000000000000000 ) ) ;
#785 = CARTESIAN_POINT ( 'NONE',  ( -1.067641779222573639, 0.6107141540073636188, -0.09374999999999998612 ) ) ;
#786 = FACE_OUTER_BOUND ( 'NONE', #5326, .T. ) ;
#787 = VERTEX_POINT ( 'NONE', #2664 ) ;
#788 = B_SPLINE_CURVE_WITH_KNOTS ( 'NONE', 3,
 ( #3831, #2630, #1405, #5724, #793, #891 ),
 .UNSPECIFIED., .F., .F.,
 ( 4, 2, 4 ),
 ( 0.0008157146336201673373, 0.007786668999356947084, 0.01475762336509372705 ),
 .UNSPECIFIED. ) ;
#789 = VERTEX_POINT ( 'NONE', #3789 ) ;
#790 = CARTESIAN_POINT ( 'NONE',  ( 1.347111479062088626E-17, 1.362500000000000044, -0.1100000000000000006 ) ) ;
#791 = CARTESIAN_POINT ( 'NONE',  ( -0.1250000000000000000, 0.5625000000000000000, -0.03125000000000000000 ) ) ;
#792 = DATE_AND_TIME ( #5798, #2913 ) ;
#793 = CARTESIAN_POINT ( 'NONE',  ( 1.821163076082948917, 1.492795972680864169, -0.07459452442999962851 ) ) ;
#794 = CARTESIAN_POINT ( 'NONE',  ( -1.067641779222573639, 0.6107141540073635078, -0.1250000000000000000 ) ) ;
#795 = PRODUCT ( 'MAS-157', 'MAS-157', '', ( #6934 ) ) ;
#796 = VERTEX_POINT ( 'NONE', #6293 ) ;
#797 =( REPRESENTATION_RELATIONSHIP ('NONE','NONE', #4195, #2298 ) REPRESENTATION_RELATIONSHIP_WITH_TRANSFORMATION ( #7436 )SHAPE_REPRESENTATION_RELATIONSHIP( ) );
#798 = DIRECTION ( 'NONE',  ( 0.000000000000000000, 0.000000000000000000, -1.000000000000000000 ) ) ;
#799 = ORIENTED_EDGE ( 'NONE', *, *, #5540, .F. ) ;
#800 = DIRECTION ( 'NONE',  ( -0.6157549048526697044, 0.7879377495398223186, 0.000000000000000000 ) ) ;
#801 = LINE ( 'NONE', #2686, #4540 ) ;
#802 = PLANE ( 'NONE',  #7617 ) ;
#803 = B_SPLINE_CURVE_WITH_KNOTS ( 'NONE', 3,
 ( #1064, #1682, #2833, #7788 ),
 .UNSPECIFIED., .F., .F.,
 ( 4, 4 ),
 ( 0.000000000000000000, 0.001713611390986142201 ),
 .UNSPECIFIED. ) ;
#804 = CYLINDRICAL_SURFACE ( 'NONE', #6206, 0.1250000000000000000 ) ;
#805 = LOCAL_TIME ( 14, 45, 32.00000000000000000, #7183 ) ;
#806 = CARTESIAN_POINT ( 'NONE',  ( 1.761728046479479337, 1.406920720071850539, 0.1725519765195418775 ) ) ;
#807 = CC_DESIGN_APPROVAL ( #4952, ( #3600 ) ) ;
#808 = DIRECTION ( 'NONE',  ( -0.7879377495398141029, -0.6157549048526800295, 0.000000000000000000 ) ) ;
#809 = PERSON_AND_ORGANIZATION ( #4735, #6190 ) ;
#810 = VERTEX_POINT ( 'NONE', #3168 ) ;
#811 = DIRECTION ( 'NONE',  ( 0.000000000000000000, 0.000000000000000000, -1.000000000000000000 ) ) ;
#812 = CARTESIAN_POINT ( 'NONE',  ( 0.3037072441740230055, -0.3811681129206500596, 8.812699745186523597E-17 ) ) ;
#813 = VERTEX_POINT ( 'NONE', #5122 ) ;
#814 = VECTOR ( 'NONE', #3519, 39.37007874015748143 ) ;
#815 = CARTESIAN_POINT ( 'NONE',  ( 1.475891671935536609, 0.7226544316391472211, -0.1849999999999999978 ) ) ;
#816 = ADVANCED_FACE ( 'NONE', ( #7623 ), #6538, .F. ) ;
#817 = LOCAL_TIME ( 14, 45, 32.00000000000000000, #998 ) ;
#818 = AXIS2_PLACEMENT_3D ( 'NONE', #2222, #372, #1038 ) ;
#819 = LINE ( 'NONE', #5823, #4777 ) ;
#820 = CARTESIAN_POINT ( 'NONE',  ( 6.185915932927993133, 0.4597367884986652831, 0.1250000000000000278 ) ) ;
#821 = COORDINATED_UNIVERSAL_TIME_OFFSET ( 0, 0, .AHEAD. ) ;
#822 = VERTEX_POINT ( 'NONE', #955 ) ;
#823 = EDGE_CURVE ( 'NONE', #4706, #787, #5910, .T. ) ;
#824 = CARTESIAN_POINT ( 'NONE',  ( 0.6597999294535048520, -0.04777128394798136474, 0.07449999999999999678 ) ) ;
#825 = LOCAL_TIME ( 14, 45, 32.00000000000000000, #4045 ) ;
#826 = CARTESIAN_POINT ( 'NONE',  ( 1.400692579912386826, 1.149720402407784059, 0.2179999999999999438 ) ) ;
#827 = ADVANCED_FACE ( 'NONE', ( #7752 ), #2098, .F. ) ;
#828 = CIRCLE ( 'NONE', #439, 0.1487499999999999933 ) ;
#829 = EDGE_CURVE ( 'NONE', #4837, #3183, #2082, .T. ) ;
#830 = PRODUCT_DEFINITION ( 'UNKNOWN', '', #4603, #5394 ) ;
#831 = CIRCLE ( 'NONE', #5683, 0.2499400561648078278 ) ;
#832 = EDGE_CURVE ( 'NONE', #3919, #4588, #5185, .T. ) ;
#833 = AXIS2_PLACEMENT_3D ( 'NONE', #2345, #4971, #506 ) ;
#834 = CARTESIAN_POINT ( 'NONE',  ( 1.684866161243239846, 1.178252195112418299, -0.1039999999999998703 ) ) ;
#835 = COORDINATED_UNIVERSAL_TIME_OFFSET ( 0, 0, .AHEAD. ) ;
#836 = LINE ( 'NONE', #3530, #1540 ) ;
#837 = FACE_OUTER_BOUND ( 'NONE', #3839, .T. ) ;
#838 = EDGE_CURVE ( 'NONE', #2970, #6487, #342, .T. ) ;
#839 = ORIENTED_EDGE ( 'NONE', *, *, #6424, .T. ) ;
#840 = EDGE_LOOP ( 'NONE', ( #3164, #71, #3687 ) ) ;
#841 = ORIENTED_EDGE ( 'NONE', *, *, #3148, .T. ) ;
#842 = CC_DESIGN_APPROVAL ( #6203, ( #448 ) ) ;
#843 = AXIS2_PLACEMENT_3D ( 'NONE', #5806, #1370, #2637 ) ;
#844 = ORIENTED_EDGE ( 'NONE', *, *, #3027, .T. ) ;
#845 = VERTEX_POINT ( 'NONE', #3984 ) ;
#846 = VERTEX_POINT ( 'NONE', #2141 ) ;
#847 = CARTESIAN_POINT ( 'NONE',  ( 0.000000000000000000, 1.362500000000000044, 0.000000000000000000 ) ) ;
#848 = ORIENTED_EDGE ( 'NONE', *, *, #4685, .T. ) ;
#849 = CARTESIAN_POINT ( 'NONE',  ( 1.726550314240142381, 1.368787266291294991, 0.1934252906403959582 ) ) ;
#850 = CARTESIAN_POINT ( 'NONE',  ( 3.659299226295303686, -8.245510427152350275, 0.1250000000000004441 ) ) ;
#851 = VECTOR ( 'NONE', #433, 39.37007874015748143 ) ;
#852 = VECTOR ( 'NONE', #204, 39.37007874015748143 ) ;
#853 = DIRECTION ( 'NONE',  ( 1.000000000000000000, 0.000000000000000000, 0.000000000000000000 ) ) ;
#854 = CARTESIAN_POINT ( 'NONE',  ( 0.2796912674001651444, -4.528516545235133250, -0.05999999999999999778 ) ) ;
#855 = AXIS2_PLACEMENT_3D ( 'NONE', #4627, #5253, #7736 ) ;
#856 = AXIS2_PLACEMENT_3D ( 'NONE', #1926, #6841, #3852 ) ;
#857 = EDGE_CURVE ( 'NONE', #1913, #7141, #6490, .T. ) ;
#858 = CARTESIAN_POINT ( 'NONE',  ( 1.840267422809780173, 1.485682443985806067, 0.03416929312143927866 ) ) ;
#859 = CARTESIAN_POINT ( 'NONE',  ( -1.499610808650658100, -1.013166758633947007, 0.3125000000000000000 ) ) ;
#860 = APPLICATION_PROTOCOL_DEFINITION ( 'international standard', 'config_control_design', 1994, #4059 ) ;
#861 = ORIENTED_EDGE ( 'NONE', *, *, #4938, .T. ) ;
#862 = CARTESIAN_POINT ( 'NONE',  ( 1.301676237712382722, 1.089389786036094376, -0.1088174584421244540 ) ) ;
#863 = CARTESIAN_POINT ( 'NONE',  ( 0.3210139061311759745, -0.3692105794741389335, 0.002757220755949914542 ) ) ;
#864 = AXIS2_PLACEMENT_3D ( 'NONE', #2591, #6363, #5714 ) ;
#865 = ORIENTED_EDGE ( 'NONE', *, *, #328, .T. ) ;
#866 = CARTESIAN_POINT ( 'NONE',  ( 1.107456280057753872, 1.514518649799285299, -0.2121970708455140908 ) ) ;
#867 = AXIS2_PLACEMENT_3D ( 'NONE', #41, #2540, #7545 ) ;
#868 = LINE ( 'NONE', #1906, #6090 ) ;
#869 = MANIFOLD_SOLID_BREP ( 'Cut-Extrude1', #4398 ) ;
#870 = DIRECTION ( 'NONE',  ( 0.000000000000000000, 0.000000000000000000, -1.000000000000000000 ) ) ;
#871 = APPROVAL_DATE_TIME ( #2871, #424 ) ;
#872 = EDGE_CURVE ( 'NONE', #445, #1342, #6505, .T. ) ;
#873 = VERTEX_POINT ( 'NONE', #7144 ) ;
#874 = TOROIDAL_SURFACE ( 'NONE', #2041, 0.1255000000000000282, 0.06199999999999999956 ) ;
#875 = CIRCLE ( 'NONE', #2054, 0.1875000000000000278 ) ;
#876 = CARTESIAN_POINT ( 'NONE',  ( -0.1054677083281892608, 0.000000000000000000, 0.03125000000000000000 ) ) ;
#877 = PRODUCT_DEFINITION_SHAPE ( 'NONE', 'NONE',  #172 ) ;
#878 = CARTESIAN_POINT ( 'NONE',  ( 2.204364238465235822E-17, 1.050000000000000044, 0.1799999999999999933 ) ) ;
#879 = CIRCLE ( 'NONE', #356, 0.2149999999999995803 ) ;
#880 = VERTEX_POINT ( 'NONE', #1000 ) ;
#881 = ORIENTED_EDGE ( 'NONE', *, *, #7926, .T. ) ;
#882 = EDGE_CURVE ( 'NONE', #6669, #6611, #6240, .T. ) ;
#883 = DIRECTION ( 'NONE',  ( 9.121065767255463271E-17, 5.551115123125732782E-17, 1.000000000000000000 ) ) ;
#884 = EDGE_CURVE ( 'NONE', #4081, #6939, #2040, .T. ) ;
#885 = ORIENTED_EDGE ( 'NONE', *, *, #5348, .F. ) ;
#886 = ADVANCED_FACE ( 'NONE', ( #5263 ), #1526, .T. ) ;
#887 = DIRECTION ( 'NONE',  ( 0.000000000000000000, -0.000000000000000000, 1.000000000000000000 ) ) ;
#888 = ADVANCED_FACE ( 'NONE', ( #5380 ), #2826, .T. ) ;
#889 = CARTESIAN_POINT ( 'NONE',  ( -4.882388066182516084, 5.670153330992327767, 0.3125000000000000000 ) ) ;
#890 = PERSON_AND_ORGANIZATION ( #238, #4645 ) ;
#891 = CARTESIAN_POINT ( 'NONE',  ( 1.877688265130482037, 1.420950500079102286, -0.07807135826935437950 ) ) ;
#892 = CARTESIAN_POINT ( 'NONE',  ( -0.03125000000000000000, 0.000000000000000000, 0.000000000000000000 ) ) ;
#893 = ORIENTED_EDGE ( 'NONE', *, *, #3081, .T. ) ;
#894 = TOROIDAL_SURFACE ( 'NONE', #2581, 0.1255000000000000282, 0.06199999999999999956 ) ;
#895 = ORIENTED_EDGE ( 'NONE', *, *, #598, .T. ) ;
#896 = CIRCLE ( 'NONE', #1543, 0.1100000000000000006 ) ;
#897 = CC_DESIGN_DATE_AND_TIME_ASSIGNMENT ( #6659, #2850, ( #6696 ) ) ;
#898 = VERTEX_POINT ( 'NONE', #406 ) ;
#899 = EDGE_CURVE ( 'NONE', #3428, #1559, #924, .T. ) ;
#900 = ADVANCED_FACE ( 'NONE', ( #5461 ), #7949, .F. ) ;
#901 = ORIENTED_EDGE ( 'NONE', *, *, #2135, .F. ) ;
#902 = ORIENTED_EDGE ( 'NONE', *, *, #3846, .T. ) ;
#903 = DIRECTION ( 'NONE',  ( 0.7498009116086189474, -0.6531728565937869879, 0.1056589435873569599 ) ) ;
#904 = DESIGN_CONTEXT ( 'detailed design', #4059, 'design' ) ;
#905 = ORIENTED_EDGE ( 'NONE', *, *, #382, .T. ) ;
#906 = EDGE_CURVE ( 'NONE', #140, #2262, #7410, .T. ) ;
#907 = CARTESIAN_POINT ( 'NONE',  ( 1.664570443216303763, 1.333357566009973905, 0.2227136479326053131 ) ) ;
#908 = CARTESIAN_POINT ( 'NONE',  ( 1.347111479062088626E-17, 1.425000000000000044, -0.1100000000000000006 ) ) ;
#909 = DIRECTION ( 'NONE',  ( 0.000000000000000000, 0.000000000000000000, 1.000000000000000000 ) ) ;
#910 = CARTESIAN_POINT ( 'NONE',  ( 0.6645694204159616758, 0.008319420416198241783, 0.000000000000000000 ) ) ;
#911 = ORIENTED_EDGE ( 'NONE', *, *, #5030, .T. ) ;
#912 = CARTESIAN_POINT ( 'NONE',  ( 1.494536332678459090, 1.857624994339484470, 0.06788303539822813926 ) ) ;
#913 = CARTESIAN_POINT ( 'NONE',  ( 0.000000000000000000, 1.081250000000000044, -0.2425000000000000211 ) ) ;
#914 = DATE_AND_TIME ( #4551, #1201 ) ;
#915 = DIRECTION ( 'NONE',  ( -0.000000000000000000, -0.000000000000000000, 1.000000000000000000 ) ) ;
#916 = CARTESIAN_POINT ( 'NONE',  ( 6.185915932927993133, 0.4597367884986685582, 0.000000000000000000 ) ) ;
#917 = ORIENTED_EDGE ( 'NONE', *, *, #3885, .F. ) ;
#918 = CARTESIAN_POINT ( 'NONE',  ( 1.351681538574651675, 1.071232595603015980, -0.1189673409015081368 ) ) ;
#919 = DIRECTION ( 'NONE',  ( -1.000000000000000000, 0.000000000000000000, 0.000000000000000000 ) ) ;
#920 = DIRECTION ( 'NONE',  ( 1.000000000000000000, 0.000000000000000000, -0.000000000000000000 ) ) ;
#921 = DATE_TIME_ROLE ( 'classification_date' ) ;
#922 = ORIENTED_EDGE ( 'NONE', *, *, #5339, .T. ) ;
#923 = EDGE_LOOP ( 'NONE', ( #5142, #7808, #3442, #6800, #1295 ) ) ;
#924 = LINE ( 'NONE', #2186, #5972 ) ;
#925 = FACE_OUTER_BOUND ( 'NONE', #6036, .T. ) ;
#926 = ORIENTED_EDGE ( 'NONE', *, *, #6693, .T. ) ;
#927 = EDGE_LOOP ( 'NONE', ( #252, #2623, #986, #2339 ) ) ;
#928 = DIRECTION ( 'NONE',  ( -1.000000000000000000, -0.000000000000000000, -0.000000000000000000 ) ) ;
#929 = CARTESIAN_POINT ( 'NONE',  ( -0.02691660025194390557, -0.4609452288429354838, 0.2500000000000001110 ) ) ;
#930 = APPROVAL_STATUS ( 'not_yet_approved' ) ;
#931 = CARTESIAN_POINT ( 'NONE',  ( -6.110602001756019419, -1.404684638105634820, 0.3125000000000000000 ) ) ;
#932 = ORIENTED_EDGE ( 'NONE', *, *, #1171, .F. ) ;
#933 = ORIENTED_EDGE ( 'NONE', *, *, #5244, .F. ) ;
#934 = FACE_OUTER_BOUND ( 'NONE', #142, .T. ) ;
#935 = ORIENTED_EDGE ( 'NONE', *, *, #4194, .T. ) ;
#936 = PERSON ( 'NAUO-PER4', 'UNSPECIFIED', 'UNSPECIFIED', ('UNSPECIFIED'), ('UNSPECIFIED'), ('UNSPECIFIED') ) ;
#937 = DIRECTION ( 'NONE',  ( 0.000000000000000000, 0.000000000000000000, -1.000000000000000000 ) ) ;
#938 = DIRECTION ( 'NONE',  ( -0.7540216022612858948, 0.6568496200222110337, 0.000000000000000000 ) ) ;
#939 = ADVANCED_FACE ( 'NONE', ( #1068, #4884 ), #4311, .T. ) ;
#940 = LINE ( 'NONE', #7171, #1865 ) ;
#941 = CARTESIAN_POINT ( 'NONE',  ( 0.000000000000000000, 0.000000000000000000, 0.06199999999999999956 ) ) ;
#942 = EDGE_CURVE ( 'NONE', #3574, #2815, #3618, .T. ) ;
#943 = ORIENTED_EDGE ( 'NONE', *, *, #382, .F. ) ;
#944 = FACE_OUTER_BOUND ( 'NONE', #1198, .T. ) ;
#945 = CC_DESIGN_PERSON_AND_ORGANIZATION_ASSIGNMENT ( #6390, #8059, ( #418 ) ) ;
#946 = ADVANCED_FACE ( 'NONE', ( #4848 ), #3569, .T. ) ;
#947 = DIRECTION ( 'NONE',  ( -0.000000000000000000, -0.000000000000000000, 1.000000000000000000 ) ) ;
#948 = EDGE_LOOP ( 'NONE', ( #3804, #3916, #5726, #3982, #2863, #4641 ) ) ;
#949 = FACE_BOUND ( 'NONE', #6261, .T. ) ;
#950 = DIRECTION ( 'NONE',  ( 1.000000000000000000, 0.000000000000000000, 0.000000000000000000 ) ) ;
#951 = CARTESIAN_POINT ( 'NONE',  ( 1.491280890329322872, 1.855080942356710949, -0.01135997346352945678 ) ) ;
#952 = SHAPE_DEFINITION_REPRESENTATION ( #2839, #3360 ) ;
#953 = EDGE_LOOP ( 'NONE', ( #6127, #848, #434, #2227 ) ) ;
#954 = AXIS2_PLACEMENT_3D ( 'NONE', #7532, #6384, #1258 ) ;
#955 = CARTESIAN_POINT ( 'NONE',  ( -1.204376266962890796, -0.2040480809676099017, 0.03199999999999999373 ) ) ;
#956 = APPROVAL_PERSON_ORGANIZATION ( #2954, #8089, #1717 ) ;
#957 = CARTESIAN_POINT ( 'NONE',  ( -0.06250000000000000000, 0.000000000000000000, 0.1250000000000000278 ) ) ;
#958 = APPROVAL_PERSON_ORGANIZATION ( #6913, #5548, #4485 ) ;
#959 = ORIENTED_EDGE ( 'NONE', *, *, #6499, .T. ) ;
#960 = EDGE_LOOP ( 'NONE', ( #6283, #7111, #597, #7336 ) ) ;
#961 = VECTOR ( 'NONE', #5920, 39.37007874015748143 ) ;
#962 = ORIENTED_EDGE ( 'NONE', *, *, #2079, .T. ) ;
#963 = VERTEX_POINT ( 'NONE', #6808 ) ;
#964 =( NAMED_UNIT ( * ) SI_UNIT ( $, .STERADIAN. ) SOLID_ANGLE_UNIT ( ) );
#965 = ORIENTED_EDGE ( 'NONE', *, *, #1887, .T. ) ;
#966 = CARTESIAN_POINT ( 'NONE',  ( 1.142655413120957197, 0.6307864494084283180, 0.03199999999999999373 ) ) ;
#967 = CARTESIAN_POINT ( 'NONE',  ( 1.414726328521486387, 1.163888030567411302, 0.2500000000000000000 ) ) ;
#968 = CALENDAR_DATE ( 2026, 9, 10 ) ;
#969 = CARTESIAN_POINT ( 'NONE',  ( 0.000000000000000000, 1.393749999999999822, 0.000000000000000000 ) ) ;
#970 = AXIS2_PLACEMENT_3D ( 'NONE', #5204, #1587, #2168 ) ;
#971 = ORIENTED_EDGE ( 'NONE', *, *, #3093, .F. ) ;
#972 = ORIENTED_EDGE ( 'NONE', *, *, #2669, .F. ) ;
#973 = AXIS2_PLACEMENT_3D ( 'NONE', #5546, #5591, #1196 ) ;
#974 = DIRECTION ( 'NONE',  ( -0.000000000000000000, 0.000000000000000000, 1.000000000000000000 ) ) ;
#975 = UNCERTAINTY_MEASURE_WITH_UNIT (LENGTH_MEASURE( 1.000000000000000082E-05 ), #4074, 'distance_accuracy_value', 'NONE');
#976 = CARTESIAN_POINT ( 'NONE',  ( -1.052129263295328521, 0.6378420796487936917, -0.09374999999999998612 ) ) ;
#977 = CARTESIAN_POINT ( 'NONE',  ( 4.390472339057043705, -2.510390028880330249, -0.09374999999999998612 ) ) ;
#978 = DIRECTION ( 'NONE',  ( 0.000000000000000000, 1.000000000000000000, 0.000000000000000000 ) ) ;
#979 = TOROIDAL_SURFACE ( 'NONE', #5949, 0.2923589946935198913, 0.03200000000000000067 ) ;
#980 = CARTESIAN_POINT ( 'NONE',  ( 1.258764021883149731, 1.079418902353951548, -0.03540237178041891197 ) ) ;
#981 = AXIS2_PLACEMENT_3D ( 'NONE', #1164, #7442, #6860 ) ;
#982 = ORIENTED_EDGE ( 'NONE', *, *, #4143, .T. ) ;
#983 = CARTESIAN_POINT ( 'NONE',  ( 3.672767723898985537, -8.314396374632453401, -0.1250000000000000000 ) ) ;
#984 = CARTESIAN_POINT ( 'NONE',  ( 1.536251789383608735, 1.851359936419108676, -0.007784679637053777863 ) ) ;
#985 = EDGE_CURVE ( 'NONE', #6844, #5923, #2953, .T. ) ;
#986 = ORIENTED_EDGE ( 'NONE', *, *, #636, .T. ) ;
#987 = DIRECTION ( 'NONE',  ( 0.4606913525677331367, 0.8875604078987031631, 0.000000000000000000 ) ) ;
#988 = ORIENTED_EDGE ( 'NONE', *, *, #2235, .F. ) ;
#989 = EDGE_CURVE ( 'NONE', #2155, #7764, #3001, .T. ) ;
#990 = DIRECTION ( 'NONE',  ( 0.000000000000000000, 0.000000000000000000, 1.000000000000000000 ) ) ;
#991 = CIRCLE ( 'NONE', #7523, 0.1150000000000000050 ) ;
#992 = CIRCLE ( 'NONE', #5438, 0.1204106507132265275 ) ;
#993 = EDGE_CURVE ( 'NONE', #2507, #5382, #1408, .T. ) ;
#994 = EDGE_CURVE ( 'NONE', #5472, #5976, #1155, .T. ) ;
#995 = CARTESIAN_POINT ( 'NONE',  ( -1.204118949239847192, -0.2049124047817365846, 0.02346499912907216642 ) ) ;
#996 = CARTESIAN_POINT ( 'NONE',  ( 1.517292316521555051, 1.875408262972374729, -0.04789697820786732035 ) ) ;
#997 = VECTOR ( 'NONE', #1776, 39.37007874015748143 ) ;
#998 = COORDINATED_UNIVERSAL_TIME_OFFSET ( 0, 0, .AHEAD. ) ;
#999 = ORIENTED_EDGE ( 'NONE', *, *, #123, .F. ) ;
#1000 = CARTESIAN_POINT ( 'NONE',  ( -0.1875000000000000278, 0.000000000000000000, 0.06300000000000000044 ) ) ;
#1001 = CARTESIAN_POINT ( 'NONE',  ( 1.503810987132070176, 1.221025632701057795, 0.2329445735574367515 ) ) ;
#1002 = ORIENTED_EDGE ( 'NONE', *, *, #5487, .T. ) ;
#1003 = CIRCLE ( 'NONE', #7916, 0.1100000000000000006 ) ;
#1004 = VERTEX_POINT ( 'NONE', #4926 ) ;
#1005 = CIRCLE ( 'NONE', #7924, 0.3099999999999745737 ) ;
#1006 = VERTEX_POINT ( 'NONE', #499 ) ;
#1007 = DIRECTION ( 'NONE',  ( 1.000000000000000000, 0.000000000000000000, 0.000000000000000000 ) ) ;
#1008 = FACE_OUTER_BOUND ( 'NONE', #6416, .T. ) ;
#1009 = LINE ( 'NONE', #2309, #6101 ) ;
#1010 = AXIS2_PLACEMENT_3D ( 'NONE', #3202, #6395, #4556 ) ;
#1011 = ORIENTED_EDGE ( 'NONE', *, *, #6995, .F. ) ;
#1012 = ORIENTED_EDGE ( 'NONE', *, *, #5031, .F. ) ;
#1013 = AXIS2_PLACEMENT_3D ( 'NONE', #7554, #2377, #4358 ) ;
#1014 = DIRECTION ( 'NONE',  ( 1.000000000000000000, 0.000000000000000000, 0.000000000000000000 ) ) ;
#1016 = LINE ( 'NONE', #4702, #7792 ) ;
#1015 = CIRCLE ( 'NONE', #2448, 0.03200000000000001454 ) ;
#1017 = DIRECTION ( 'NONE',  ( 0.6568496200222107007, 0.7540216022612863389, -0.000000000000000000 ) ) ;
#1018 = VERTEX_POINT ( 'NONE', #534 ) ;
#1019 = ORIENTED_EDGE ( 'NONE', *, *, #5646, .F. ) ;
#1020 = LINE ( 'NONE', #6630, #814 ) ;
#1021 = CARTESIAN_POINT ( 'NONE',  ( 1.492515782973968363, 1.856045982048426746, -0.05383208248535607116 ) ) ;
#1022 = CIRCLE ( 'NONE', #4822, 0.2704878104020023710 ) ;
#1023 = AXIS2_PLACEMENT_3D ( 'NONE', #1264, #1885, #3030 ) ;
#1024 = DIRECTION ( 'NONE',  ( 0.000000000000000000, 1.000000000000000000, 0.000000000000000000 ) ) ;
#1025 = DIRECTION ( 'NONE',  ( 1.000000000000000000, 0.000000000000000000, 0.000000000000000000 ) ) ;
#1026 = LINE ( 'NONE', #1101, #5715 ) ;
#1027 = ORIENTED_EDGE ( 'NONE', *, *, #5349, .F. ) ;
#1028 = DIRECTION ( 'NONE',  ( 0.000000000000000000, 1.000000000000000000, 0.000000000000000000 ) ) ;
#1029 = EDGE_CURVE ( 'NONE', #5193, #2815, #7982, .T. ) ;
#1030 = ADVANCED_FACE ( 'NONE', ( #2369 ), #4275, .F. ) ;
#1031 = CARTESIAN_POINT ( 'NONE',  ( 0.6597999294535048520, -0.01652128394798136821, 0.07449999999999999678 ) ) ;
#1032 = DIRECTION ( 'NONE',  ( 0.000000000000000000, 1.000000000000000000, -0.000000000000000000 ) ) ;
#1033 = SHAPE_DEFINITION_REPRESENTATION ( #877, #2774 ) ;
#1034 = ORIENTED_EDGE ( 'NONE', *, *, #6551, .F. ) ;
#1035 = DIRECTION ( 'NONE',  ( 0.000000000000000000, 0.000000000000000000, -1.000000000000000000 ) ) ;
#1036 = CARTESIAN_POINT ( 'NONE',  ( -0.1250000000000000000, 0.5625000000000000000, 0.03125000000000000000 ) ) ;
#1037 = CC_DESIGN_PERSON_AND_ORGANIZATION_ASSIGNMENT ( #3695, #531, ( #3550 ) ) ;
#1038 = DIRECTION ( 'NONE',  ( 1.000000000000000000, 0.000000000000000000, 0.000000000000000000 ) ) ;
#1039 = EDGE_CURVE ( 'NONE', #1869, #4782, #3698, .T. ) ;
#1040 = EDGE_CURVE ( 'NONE', #3041, #7825, #7665, .T. ) ;
#1041 = ORIENTED_EDGE ( 'NONE', *, *, #4042, .T. ) ;
#1042 = ORIENTED_EDGE ( 'NONE', *, *, #6457, .T. ) ;
#1043 = LINE ( 'NONE', #6083, #6213 ) ;
#1044 = CARTESIAN_POINT ( 'NONE',  ( 1.417679350985660447, 1.200983401422921704, 0.2500000000000000000 ) ) ;
#1045 = DATE_AND_TIME ( #7195, #1626 ) ;
#1046 = CC_DESIGN_PERSON_AND_ORGANIZATION_ASSIGNMENT ( #4715, #7213, ( #6959 ) ) ;
#1047 = CARTESIAN_POINT ( 'NONE',  ( 0.000000000000000000, 0.6124999999999999334, 0.000000000000000000 ) ) ;
#1048 = VERTEX_POINT ( 'NONE', #1846 ) ;
#1049 = DIRECTION ( 'NONE',  ( 1.000000000000000000, 0.000000000000000000, 0.000000000000000000 ) ) ;
#1050 = DIRECTION ( 'NONE',  ( 0.04906492035527430795, -0.9987955914953422498, 0.000000000000000000 ) ) ;
#1051 = PERSON_AND_ORGANIZATION_ROLE ( 'design_owner' ) ;
#1052 = CYLINDRICAL_SURFACE ( 'NONE', #5340, 0.1150000000000000050 ) ;
#1053 = LINE ( 'NONE', #3546, #1766 ) ;
#1054 = ORIENTED_EDGE ( 'NONE', *, *, #2781, .T. ) ;
#1055 = DIRECTION ( 'NONE',  ( 0.000000000000000000, 0.000000000000000000, 1.000000000000000000 ) ) ;
#1056 = DIRECTION ( 'NONE',  ( 0.6157549048526803626, -0.7879377495398141029, 0.000000000000000000 ) ) ;
#1057 = CARTESIAN_POINT ( 'NONE',  ( -1.204376266962890796, -0.2040480809676099017, 0.2179999999999999993 ) ) ;
#1058 = CARTESIAN_POINT ( 'NONE',  ( -1.543211452806561690, 0.6927940070358462599, 0.1250000000000000000 ) ) ;
#1059 = DIRECTION ( 'NONE',  ( 0.000000000000000000, 0.000000000000000000, 1.000000000000000000 ) ) ;
#1060 = ORIENTED_EDGE ( 'NONE', *, *, #1531, .T. ) ;
#1061 = VERTEX_POINT ( 'NONE', #7902 ) ;
#1062 = CARTESIAN_POINT ( 'NONE',  ( -4.521705384338368994, -3.437882612028420048, 0.2179999999999999993 ) ) ;
#1063 = CARTESIAN_POINT ( 'NONE',  ( 0.1054677083281892608, 0.6124999999999999334, 0.03125000000000000000 ) ) ;
#1064 = CARTESIAN_POINT ( 'NONE',  ( 1.380988422954957606, 1.174934410395800821, 0.2500000000000000000 ) ) ;
#1065 = PERSON_AND_ORGANIZATION_ROLE ( 'design_owner' ) ;
#1066 = ORIENTED_EDGE ( 'NONE', *, *, #329, .T. ) ;
#1067 = CARTESIAN_POINT ( 'NONE',  ( -1.222146065255383940, -0.1443597716867830172, 0.3125000000000000000 ) ) ;
#1068 = FACE_OUTER_BOUND ( 'NONE', #7114, .T. ) ;
#1069 = PLANE ( 'NONE',  #4488 ) ;
#1070 = AXIS2_PLACEMENT_3D ( 'NONE', #3137, #7025, #2668 ) ;
#1071 = ORIENTED_EDGE ( 'NONE', *, *, #7393, .T. ) ;
#1072 = AXIS2_PLACEMENT_3D ( 'NONE', #269, #6421, #5325 ) ;
#1073 = ORIENTED_EDGE ( 'NONE', *, *, #5287, .F. ) ;
#1074 = CARTESIAN_POINT ( 'NONE',  ( 0.1054677083281892608, 0.5625000000000000000, -0.03125000000000000000 ) ) ;
#1075 = CARTESIAN_POINT ( 'NONE',  ( 0.09911377505692577083, -0.4587915400498679963, 0.2226707364275206102 ) ) ;
#1076 = APPROVAL_DATE_TIME ( #6694, #5247 ) ;
#1077 = DIRECTION ( 'NONE',  ( 6.975840231036812635E-15, -1.000000000000000000, -2.013666839457971600E-30 ) ) ;
#1078 = EDGE_CURVE ( 'NONE', #91, #6877, #4351, .T. ) ;
#1079 = VERTEX_POINT ( 'NONE', #3735 ) ;
#1080 = EDGE_CURVE ( 'NONE', #898, #3734, #5417, .T. ) ;
#1081 = AXIS2_PLACEMENT_3D ( 'NONE', #2958, #6320, #704 ) ;
#1082 = ORIENTED_EDGE ( 'NONE', *, *, #4949, .T. ) ;
#1083 = CC_DESIGN_APPROVAL ( #1278, ( #7756 ) ) ;
#1084 = CC_DESIGN_PERSON_AND_ORGANIZATION_ASSIGNMENT ( #6786, #1167, ( #4480 ) ) ;
#1085 = EDGE_CURVE ( 'NONE', #2424, #5238, #4189, .T. ) ;
#1086 = VERTEX_POINT ( 'NONE', #7581 ) ;
#1087 = CARTESIAN_POINT ( 'NONE',  ( 1.288127153466032349, 1.061753156913864515, -0.04562500015858166058 ) ) ;
#1088 = DIRECTION ( 'NONE',  ( 0.000000000000000000, -0.000000000000000000, -1.000000000000000000 ) ) ;
#1089 = VECTOR ( 'NONE', #5990, 39.37007874015748143 ) ;
#1090 = DIRECTION ( 'NONE',  ( 0.000000000000000000, 0.000000000000000000, 1.000000000000000000 ) ) ;
#1091 = COORDINATED_UNIVERSAL_TIME_OFFSET ( 0, 0, .AHEAD. ) ;
#1092 = CARTESIAN_POINT ( 'NONE',  ( 3.659299226295303686, -8.245510427152350275, 5.393636709996481038 ) ) ;
#1093 = EDGE_LOOP ( 'NONE', ( #6163, #7798, #6038, #6708 ) ) ;
#1094 = ORIENTED_EDGE ( 'NONE', *, *, #2742, .T. ) ;
#1095 = CARTESIAN_POINT ( 'NONE',  ( 0.000000000000000000, 1.393749999999999822, 0.000000000000000000 ) ) ;
#1096 = CARTESIAN_POINT ( 'NONE',  ( 0.1250000000000000278, -0.03125000000000000000, 0.06250000000000000000 ) ) ;
#1097 = AXIS2_PLACEMENT_3D ( 'NONE', #7269, #4654, #3504 ) ;
#1098 = DIRECTION ( 'NONE',  ( -0.7540216022612864499, 0.6568496200222104786, 0.000000000000000000 ) ) ;
#1099 = AXIS2_PLACEMENT_3D ( 'NONE', #1785, #3757, #3638 ) ;
#1100 = CIRCLE ( 'NONE', #1627, 0.01652128394798136474 ) ;
#1101 = CARTESIAN_POINT ( 'NONE',  ( -1.983451234524918227, 1.341543513548240529, -0.2959999999999997078 ) ) ;
#1102 = EDGE_LOOP ( 'NONE', ( #6425, #1747, #4521, #7627, #6887, #1550 ) ) ;
#1103 = ORIENTED_EDGE ( 'NONE', *, *, #6156, .T. ) ;
#1104 = DIRECTION ( 'NONE',  ( -0.8680936205257663296, 0.4964005096718443477, -0.000000000000000000 ) ) ;
#1105 = SECURITY_CLASSIFICATION ( '', '', #3745 ) ;
#1106 = CIRCLE ( 'NONE', #981, 8.633908398497672110 ) ;
#1107 = DIRECTION ( 'NONE',  ( 1.000000000000000000, 0.000000000000000000, 0.000000000000000000 ) ) ;
#1108 = CARTESIAN_POINT ( 'NONE',  ( 1.721454941643402181, 1.365050579745590298, 0.1970682748494993752 ) ) ;
#1109 = COORDINATED_UNIVERSAL_TIME_OFFSET ( 0, 0, .AHEAD. ) ;
#1110 = VERTEX_POINT ( 'NONE', #4397 ) ;
#1111 = CARTESIAN_POINT ( 'NONE',  ( -0.9280291358773672394, 0.8548654847802351631, 0.09374999999999998612 ) ) ;
#1112 = DIRECTION ( 'NONE',  ( 0.000000000000000000, 0.000000000000000000, -1.000000000000000000 ) ) ;
#1113 = VECTOR ( 'NONE', #7817, 39.37007874015748143 ) ;
#1114 = DIRECTION ( 'NONE',  ( 0.9578262852211522071, 0.000000000000000000, -0.2873478855663425535 ) ) ;
#1115 = APPLICATION_CONTEXT ( 'configuration controlled 3d designs of mechanical parts and assemblies' ) ;
#1116 = VERTEX_POINT ( 'NONE', #2050 ) ;
#1117 = AXIS2_PLACEMENT_3D ( 'NONE', #3460, #5967, #7836 ) ;
#1118 = AXIS2_PLACEMENT_3D ( 'NONE', #3683, #1917, #6183 ) ;
#1119 = CARTESIAN_POINT ( 'NONE',  ( 0.000000000000000000, 1.362500000000000044, 0.1100000000000000006 ) ) ;
#1120 =( LENGTH_UNIT ( ) NAMED_UNIT ( * ) SI_UNIT ( $, .METRE. ) );
#1121 = ORIENTED_EDGE ( 'NONE', *, *, #5895, .F. ) ;
#1122 = CARTESIAN_POINT ( 'NONE',  ( 0.000000000000000000, 1.081250000000000044, 0.000000000000000000 ) ) ;
#1123 = DATE_TIME_ROLE ( 'classification_date' ) ;
#1124 = DIRECTION ( 'NONE',  ( 0.6157549048526823610, -0.7879377495398123266, 0.000000000000000000 ) ) ;
#1125 = VERTEX_POINT ( 'NONE', #4509 ) ;
#1126 = EDGE_CURVE ( 'NONE', #1869, #796, #7148, .T. ) ;
#1127 = EDGE_CURVE ( 'NONE', #3019, #4660, #3572, .T. ) ;
#1128 = CARTESIAN_POINT ( 'NONE',  ( 1.298294415927210732, 1.066201332570530402, -0.05662632202991332159 ) ) ;
#1129 = AXIS2_PLACEMENT_3D ( 'NONE', #4218, #7455, #6717 ) ;
#1130 = CARTESIAN_POINT ( 'NONE',  ( 1.892615878912688121, 1.261282748826759059, -0.1039999999999998703 ) ) ;
#1131 = DIRECTION ( 'NONE',  ( 1.000000000000000000, 1.049151427428407716E-10, 0.000000000000000000 ) ) ;
#1132 = SECURITY_CLASSIFICATION_LEVEL ( 'unclassified' ) ;
#1133 = DIRECTION ( 'NONE',  ( 0.000000000000000000, 1.000000000000000000, 0.000000000000000000 ) ) ;
#1134 = CARTESIAN_POINT ( 'NONE',  ( 1.879749225811877533, 1.418330869987895593, -0.07819788172161412643 ) ) ;
#1135 = ORIENTED_EDGE ( 'NONE', *, *, #1127, .F. ) ;
#1136 = CIRCLE ( 'NONE', #742, 0.2499962251234248700 ) ;
#1137 = CC_DESIGN_PERSON_AND_ORGANIZATION_ASSIGNMENT ( #4284, #4238, ( #51 ) ) ;
#1138 = CIRCLE ( 'NONE', #7419, 0.03200000000000009781 ) ;
#1139 = CARTESIAN_POINT ( 'NONE',  ( 1.631407451075704174, 1.225884142284358269, 0.1986297663929937618 ) ) ;
#1140 = CARTESIAN_POINT ( 'NONE',  ( -1.855136387357835481, 0.9645206712600612464, -0.08100000000000007194 ) ) ;
#1141 = EDGE_CURVE ( 'NONE', #5314, #1559, #7503, .T. ) ;
#1142 = AXIS2_PLACEMENT_3D ( 'NONE', #7646, #5147, #7040 ) ;
#1143 = PLANE ( 'NONE',  #3737 ) ;
#1144 = FACE_OUTER_BOUND ( 'NONE', #927, .T. ) ;
#1145 = CARTESIAN_POINT ( 'NONE',  ( 0.09374999999999998612, 0.000000000000000000, 0.1250000000000000000 ) ) ;
#1146 = ORIENTED_EDGE ( 'NONE', *, *, #411, .F. ) ;
#1147 = CIRCLE ( 'NONE', #7429, 0.2500000000000000555 ) ;
#1148 = CARTESIAN_POINT ( 'NONE',  ( 0.000000000000000000, 1.425000000000000044, 0.000000000000000000 ) ) ;
#1149 = CIRCLE ( 'NONE', #4413, 0.3243589946935201418 ) ;
#1150 = DIRECTION ( 'NONE',  ( 0.000000000000000000, 0.000000000000000000, 1.000000000000000000 ) ) ;
#1151 = CARTESIAN_POINT ( 'NONE',  ( 1.804885088013157501, 1.272044176619705036, -0.1039999999999998703 ) ) ;
#1152 = CALENDAR_DATE ( 2026, 9, 10 ) ;
#1153 = ORIENTED_EDGE ( 'NONE', *, *, #412, .F. ) ;
#1154 = FACE_OUTER_BOUND ( 'NONE', #3679, .T. ) ;
#1155 = LINE ( 'NONE', #2957, #731 ) ;
#1156 = ORIENTED_EDGE ( 'NONE', *, *, #7699, .F. ) ;
#1157 = DIRECTION ( 'NONE',  ( -0.8680936205257663296, 0.4964005096718443477, 0.000000000000000000 ) ) ;
#1158 = ORIENTED_EDGE ( 'NONE', *, *, #6192, .F. ) ;
#1159 = DIRECTION ( 'NONE',  ( 0.000000000000000000, 1.000000000000000000, 0.000000000000000000 ) ) ;
#1160 = LINE ( 'NONE', #4317, #3059 ) ;
#1161 = APPROVAL_ROLE ( '' ) ;
#1162 = DIRECTION ( 'NONE',  ( 0.000000000000000000, -0.000000000000000000, -1.000000000000000000 ) ) ;
#1163 = ORIENTED_EDGE ( 'NONE', *, *, #421, .T. ) ;
#1164 = CARTESIAN_POINT ( 'NONE',  ( 3.672767464462126430, -8.314346814944791220, -0.1849999999999999978 ) ) ;
#1165 = CARTESIAN_POINT ( 'NONE',  ( 0.000000000000000000, -0.03125000000000000000, 0.000000000000000000 ) ) ;
#1166 = DIRECTION ( 'NONE',  ( -0.7879377495398141029, -0.6157549048526801405, 0.000000000000000000 ) ) ;
#1167 = PERSON_AND_ORGANIZATION_ROLE ( 'design_supplier' ) ;
#1168 = CARTESIAN_POINT ( 'NONE',  ( 1.414905630928118274, 1.059296705655214499, -0.2064098076014010408 ) ) ;
#1169 = CARTESIAN_POINT ( 'NONE',  ( 1.821814260629908144, 1.491972579020843792, -0.07464810438835918494 ) ) ;
#1170 = CARTESIAN_POINT ( 'NONE',  ( 1.449232787663330191, 1.184861245930724838, 0.2316522750340390402 ) ) ;
#1171 = EDGE_CURVE ( 'NONE', #1380, #1544, #3126, .T. ) ;
#1172 = PLANE ( 'NONE',  #174 ) ;
#1173 = EDGE_LOOP ( 'NONE', ( #7603, #7692, #7516, #3259 ) ) ;
#1174 = EDGE_LOOP ( 'NONE', ( #276, #7729, #4961, #982 ) ) ;
#1175 = CYLINDRICAL_SURFACE ( 'NONE', #1118, 0.1250000000000000000 ) ;
#1176 = DIRECTION ( 'NONE',  ( -0.000000000000000000, 0.000000000000000000, -1.000000000000000000 ) ) ;
#1177 = PLANE ( 'NONE',  #5328 ) ;
#1178 = ADVANCED_FACE ( 'NONE', ( #1270 ), #4469, .T. ) ;
#1179 = EDGE_LOOP ( 'NONE', ( #114, #1692, #343, #5866 ) ) ;
#1180 = ADVANCED_FACE ( 'NONE', ( #5663 ), #3160, .T. ) ;
#1181 = ADVANCED_FACE ( 'NONE', ( #620 ), #5776, .F. ) ;
#1182 = ORIENTED_EDGE ( 'NONE', *, *, #4192, .T. ) ;
#1183 = DIRECTION ( 'NONE',  ( 0.000000000000000000, 0.000000000000000000, 1.000000000000000000 ) ) ;
#1184 = EDGE_CURVE ( 'NONE', #661, #1476, #1914, .T. ) ;
#1185 = APPROVAL ( #3198, 'UNSPECIFIED' ) ;
#1186 = EDGE_CURVE ( 'NONE', #1576, #3933, #6108, .T. ) ;
#1187 = CARTESIAN_POINT ( 'NONE',  ( 0.8135394388118154518, 1.284829519253825492, -0.3750000000000000555 ) ) ;
#1188 = FACE_OUTER_BOUND ( 'NONE', #2753, .T. ) ;
#1189 = PERSON_AND_ORGANIZATION ( #4735, #6190 ) ;
#1190 = ORIENTED_EDGE ( 'NONE', *, *, #1680, .F. ) ;
#1191 = DIRECTION ( 'NONE',  ( 1.000000000000000000, -0.000000000000000000, -0.000000000000000000 ) ) ;
#1192 = CARTESIAN_POINT ( 'NONE',  ( 1.475891671935536831, 0.7226544316391477762, -0.1120558261758407559 ) ) ;
#1193 = ORIENTED_EDGE ( 'NONE', *, *, #3385, .T. ) ;
#1194 = CARTESIAN_POINT ( 'NONE',  ( 1.101712734284013395, 0.9160746524671463664, 0.03199999999999999373 ) ) ;
#1195 = CARTESIAN_POINT ( 'NONE',  ( 1.859753234433174418, 1.471617347716406288, -0.009971652696953780398 ) ) ;
#1196 = DIRECTION ( 'NONE',  ( -0.6157549048526697044, 0.7879377495398223186, 0.000000000000000000 ) ) ;
#1197 = CARTESIAN_POINT ( 'NONE',  ( -1.047725383040473579, -0.7302344931468570666, 0.2500000000000000555 ) ) ;
#1198 = EDGE_LOOP ( 'NONE', ( #3456, #7345 ) ) ;
#1199 = AXIS2_PLACEMENT_3D ( 'NONE', #3254, #5795, #1360 ) ;
#1200 = VERTEX_POINT ( 'NONE', #1345 ) ;
#1201 = LOCAL_TIME ( 14, 45, 32.00000000000000000, #2047 ) ;
#1202 = LINE ( 'NONE', #2387, #3603 ) ;
#1203 = CARTESIAN_POINT ( 'NONE',  ( 0.2796912674001651444, -4.528516545235133250, 0.3125000000000000000 ) ) ;
#1204 = CARTESIAN_POINT ( 'NONE',  ( 0.07611279676787391368, -0.4615777240268290615, 0.01842339291575492005 ) ) ;
#1205 = PERSON_AND_ORGANIZATION ( #4735, #6190 ) ;
#1206 = CYLINDRICAL_SURFACE ( 'NONE', #5337, 0.2499400561648078278 ) ;
#1207 = CARTESIAN_POINT ( 'NONE',  ( 1.676600392854198152, 1.675569901472168111, -0.06304405137341999310 ) ) ;
#1208 = AXIS2_PLACEMENT_3D ( 'NONE', #5107, #6276, #650 ) ;
#1209 = ORIENTED_EDGE ( 'NONE', *, *, #7496, .F. ) ;
#1210 = CARTESIAN_POINT ( 'NONE',  ( 1.681471845429138634, 1.360654782462170198, 0.2349444525762485469 ) ) ;
#1211 = PRODUCT_DEFINITION_FORMATION_WITH_SPECIFIED_SOURCE ( 'ANY', '', #4024, .NOT_KNOWN. ) ;
#1212 = CIRCLE ( 'NONE', #2260, 0.1255000000000000282 ) ;
#1213 = ADVANCED_FACE ( 'NONE', ( #157 ), #7540, .T. ) ;
#1214 = CARTESIAN_POINT ( 'NONE',  ( 0.07000000000000002054, -0.03125000000000000000, 0.8125000000000000000 ) ) ;
#1215 = PLANE ( 'NONE',  #5588 ) ;
#1216 = EDGE_CURVE ( 'NONE', #1079, #5222, #351, .T. ) ;
#1217 = CARTESIAN_POINT ( 'NONE',  ( 1.812419000491751309, 1.462705014722680996, 0.09539854745190586016 ) ) ;
#1218 = VERTEX_POINT ( 'NONE', #7010 ) ;
#1219 = AXIS2_PLACEMENT_3D ( 'NONE', #980, #4058, #7849 ) ;
#1220 = CARTESIAN_POINT ( 'NONE',  ( 6.068104892000602213, -0.009251957739379222667, 0.1849999999999999978 ) ) ;
#1221 =( REPRESENTATION_RELATIONSHIP ('NONE','NONE', #4195, #6436 ) REPRESENTATION_RELATIONSHIP_WITH_TRANSFORMATION ( #1282 )SHAPE_REPRESENTATION_RELATIONSHIP( ) );
#1222 = ADVANCED_FACE ( 'NONE', ( #7660 ), #7021, .F. ) ;
#1223 = EDGE_CURVE ( 'NONE', #2029, #6549, #4804, .T. ) ;
#1224 = ORIENTED_EDGE ( 'NONE', *, *, #6688, .T. ) ;
#1225 = DIRECTION ( 'NONE',  ( 1.000000000000000000, 0.000000000000000000, 0.000000000000000000 ) ) ;
#1226 = CARTESIAN_POINT ( 'NONE',  ( 1.571814533976804151, 1.273076930690908437, 0.2372021369714001904 ) ) ;
#1227 = COORDINATED_UNIVERSAL_TIME_OFFSET ( 0, 0, .AHEAD. ) ;
#1228 = EDGE_LOOP ( 'NONE', ( #2359, #4248, #5874, #105 ) ) ;
#1229 = DIRECTION ( 'NONE',  ( -0.6021462665530982195, 0.7983857925064579142, 0.000000000000000000 ) ) ;
#1230 = DIRECTION ( 'NONE',  ( 0.000000000000000000, 0.000000000000000000, -1.000000000000000000 ) ) ;
#1231 = VERTEX_POINT ( 'NONE', #776 ) ;
#1232 = CARTESIAN_POINT ( 'NONE',  ( 1.697621308141715746, 1.379869104482623454, 0.2130385109652204456 ) ) ;
#1233 = APPROVAL ( #3089, 'UNKNOWN' ) ;
#1234 = CIRCLE ( 'NONE', #1352, 0.03124999999999999306 ) ;
#1235 = EDGE_CURVE ( 'NONE', #340, #3734, #7053, .T. ) ;
#1236 = EDGE_CURVE ( 'NONE', #4072, #7994, #246, .T. ) ;
#1237 = ORIENTED_EDGE ( 'NONE', *, *, #6506, .F. ) ;
#1238 = VERTEX_POINT ( 'NONE', #2783 ) ;
#1239 = LINE ( 'NONE', #503, #6367 ) ;
#1240 = DIRECTION ( 'NONE',  ( -0.7879377495398141029, -0.6157549048526800295, -0.000000000000000000 ) ) ;
#1241 = DIRECTION ( 'NONE',  ( -1.000000000000000000, -6.975840231036812635E-15, 0.000000000000000000 ) ) ;
#1242 = AXIS2_PLACEMENT_3D ( 'NONE', #4527, #7029, #7634 ) ;
#1243 = CIRCLE ( 'NONE', #5048, 0.1799999999999999933 ) ;
#1244 = ORIENTED_EDGE ( 'NONE', *, *, #1432, .T. ) ;
#1245 = DIRECTION ( 'NONE',  ( 0.000000000000000000, 0.000000000000000000, 1.000000000000000000 ) ) ;
#1246 = DIRECTION ( 'NONE',  ( 0.000000000000000000, 0.000000000000000000, -1.000000000000000000 ) ) ;
#1247 = DIRECTION ( 'NONE',  ( -0.7879377495398138809, -0.6157549048526803626, 0.000000000000000000 ) ) ;
#1248 = PERSON_AND_ORGANIZATION_ROLE ( 'creator' ) ;
#1249 = DIRECTION ( 'NONE',  ( -0.4606913525677331367, -0.8875604078987033851, 0.000000000000000000 ) ) ;
#1250 = CARTESIAN_POINT ( 'NONE',  ( 0.000000000000000000, 0.000000000000000000, 0.000000000000000000 ) ) ;
#1251 = VECTOR ( 'NONE', #1535, 39.37007874015748143 ) ;
#1252 = VERTEX_POINT ( 'NONE', #3409 ) ;
#1254 = DIRECTION ( 'NONE',  ( 1.000000000000000000, 0.000000000000000000, 0.000000000000000000 ) ) ;
#1253 = AXIS2_PLACEMENT_3D ( 'NONE', #7049, #7577, #1422 ) ;
#1255 = CARTESIAN_POINT ( 'NONE',  ( 0.000000000000000000, 0.000000000000000000, 0.1100000000000000006 ) ) ;
#1256 = CIRCLE ( 'NONE', #5848, 9.004497838701050583 ) ;
#1257 = B_SPLINE_CURVE_WITH_KNOTS ( 'NONE', 3,
 ( #5005, #3619, #500, #7505, #7467, #6849, #536, #1232, #5502, #8066 ),
 .UNSPECIFIED., .F., .F.,
 ( 4, 2, 2, 2, 4 ),
 ( 0.000000000000000000, 0.001297014371279050018, 0.002594028742558100037, 0.003891043113837150055, 0.005188057485116200074 ),
 .UNSPECIFIED. ) ;
#1258 = DIRECTION ( 'NONE',  ( -0.8875604078987042733, 0.4606913525677314158, 0.000000000000000000 ) ) ;
#1259 = ORIENTED_EDGE ( 'NONE', *, *, #4440, .T. ) ;
#1260 = DIRECTION ( 'NONE',  ( -0.6157549048526802515, 0.7879377495398139919, -0.000000000000000000 ) ) ;
#1261 = VECTOR ( 'NONE', #6819, 39.37007874015748143 ) ;
#1262 = ORIENTED_EDGE ( 'NONE', *, *, #6829, .F. ) ;
#1263 = CARTESIAN_POINT ( 'NONE',  ( -0.09999999999999997780, -0.03125000000000000000, 0.8125000000000000000 ) ) ;
#1264 = CARTESIAN_POINT ( 'NONE',  ( 2.010976737284365878, 1.235749360019309684, -0.08212881570848259982 ) ) ;
#1265 = APPROVAL_STATUS ( 'not_yet_approved' ) ;
#1266 = EDGE_LOOP ( 'NONE', ( #6103, #6463, #8052, #5215 ) ) ;
#1267 = CARTESIAN_POINT ( 'NONE',  ( -1.763177565995708296, 1.070083551578370207, -0.08100000000000007194 ) ) ;
#1268 = AXIS2_PLACEMENT_3D ( 'NONE', #1946, #4454, #6949 ) ;
#1269 = VECTOR ( 'NONE', #3694, 39.37007874015748143 ) ;
#1270 = FACE_OUTER_BOUND ( 'NONE', #754, .T. ) ;
#1271 = ORIENTED_EDGE ( 'NONE', *, *, #838, .T. ) ;
#1272 = CARTESIAN_POINT ( 'NONE',  ( -3.165020334763531729, -1.163753072338894023, 0.1250000000000000000 ) ) ;
#1273 = EDGE_CURVE ( 'NONE', #2327, #1856, #3223, .T. ) ;
#1274 = EDGE_CURVE ( 'NONE', #3903, #7063, #8051, .T. ) ;
#1275 = EDGE_CURVE ( 'NONE', #3595, #3574, #4992, .T. ) ;
#1276 = CIRCLE ( 'NONE', #6643, 0.1799999999999999933 ) ;
#1277 = CARTESIAN_POINT ( 'NONE',  ( 1.550255360611296540, 0.8757063900986424843, -0.08212881570848257207 ) ) ;
#1278 = APPROVAL ( #7095, 'UNSPECIFIED' ) ;
#1279 = DIRECTION ( 'NONE',  ( 1.000000000000000000, 0.000000000000000000, 0.000000000000000000 ) ) ;
#1280 = CARTESIAN_POINT ( 'NONE',  ( 1.414905630928118274, 1.059296705655214499, -0.2064098076014010408 ) ) ;
#1281 = EDGE_CURVE ( 'NONE', #7143, #4391, #5292, .T. ) ;
#1282 = ITEM_DEFINED_TRANSFORMATION ( 'NONE', 'NONE', #6971,  #3555 ) ;
#1283 = CARTESIAN_POINT ( 'NONE',  ( 1.537918127343594454, 1.852987194258524983, 0.000000000000000000 ) ) ;
#1284 = EDGE_CURVE ( 'NONE', #4126, #4355, #5586, .T. ) ;
#1285 = ORIENTED_EDGE ( 'NONE', *, *, #4841, .F. ) ;
#1286 = CC_DESIGN_SECURITY_CLASSIFICATION ( #2562, ( #8094 ) ) ;
#1287 = CC_DESIGN_DATE_AND_TIME_ASSIGNMENT ( #8083, #6222, ( #5651 ) ) ;
#1288 = CARTESIAN_POINT ( 'NONE',  ( -1.432604426929670494, 0.8194101287839825609, 0.1250000000000000000 ) ) ;
#1289 = EDGE_CURVE ( 'NONE', #2344, #813, #364, .T. ) ;
#1290 = CARTESIAN_POINT ( 'NONE',  ( 1.580248108977379884, 1.266138851169832380, -0.1250000000000000278 ) ) ;
#1291 = EDGE_CURVE ( 'NONE', #6487, #2970, #2561, .T. ) ;
#1292 = APPROVAL_STATUS ( 'not_yet_approved' ) ;
#1293 = LINE ( 'NONE', #3802, #5861 ) ;
#1294 = LINE ( 'NONE', #1788, #5566 ) ;
#1295 = ORIENTED_EDGE ( 'NONE', *, *, #7243, .F. ) ;
#1296 = ORIENTED_EDGE ( 'NONE', *, *, #5085, .F. ) ;
#1297 = CARTESIAN_POINT ( 'NONE',  ( -0.3566525292043903339, -0.3408511508279103985, 0.1250000000000000000 ) ) ;
#1298 = DIRECTION ( 'NONE',  ( -0.9987955914953423608, -0.04906492035527378059, 0.000000000000000000 ) ) ;
#1299 = CARTESIAN_POINT ( 'NONE',  ( 0.8923633780935225079, 0.7607014108325281798, 0.03199999999999999373 ) ) ;
#1300 = VERTEX_POINT ( 'NONE', #4062 ) ;
#1301 = LINE ( 'NONE', #1419, #3838 ) ;
#1302 = ORIENTED_EDGE ( 'NONE', *, *, #378, .F. ) ;
#1303 = DIRECTION ( 'NONE',  ( 0.000000000000000000, -1.000000000000000000, 0.000000000000000000 ) ) ;
#1304 = CARTESIAN_POINT ( 'NONE',  ( 0.000000000000000000, 0.6124999999999999334, 0.000000000000000000 ) ) ;
#1305 = PERSON_AND_ORGANIZATION_ROLE ( 'classification_officer' ) ;
#1306 = ORIENTED_EDGE ( 'NONE', *, *, #7243, .T. ) ;
#1307 = DIRECTION ( 'NONE',  ( -0.6157549048526802515, 0.7879377495398142139, -0.000000000000000000 ) ) ;
#1308 = CARTESIAN_POINT ( 'NONE',  ( 0.000000000000000000, 0.000000000000000000, -0.6537499999999999423 ) ) ;
#1309 = DIRECTION ( 'NONE',  ( -0.9726399823210830631, -0.2323175946639496336, -0.000000000000000000 ) ) ;
#1310 = CARTESIAN_POINT ( 'NONE',  ( 5.983714301115758083, -0.05774751952986264397, -0.1849999999999999978 ) ) ;
#1311 = EDGE_CURVE ( 'NONE', #7782, #4068, #1631, .T. ) ;
#1312 = CARTESIAN_POINT ( 'NONE',  ( 0.7510138408322231118, -0.03124999999962550443, 0.07449999999999999678 ) ) ;
#1313 = FACE_OUTER_BOUND ( 'NONE', #6121, .T. ) ;
#1314 = ADVANCED_FACE ( 'NONE', ( #4630 ), #6431, .F. ) ;
#1315 = ORIENTED_EDGE ( 'NONE', *, *, #2586, .F. ) ;
#1316 = EDGE_CURVE ( 'NONE', #5686, #375, #5943, .T. ) ;
#1317 = ORIENTED_EDGE ( 'NONE', *, *, #1284, .F. ) ;
#1318 = CARTESIAN_POINT ( 'NONE',  ( 3.659299226295303686, -8.245510427152350275, 0.1850000000000003586 ) ) ;
#1319 = EDGE_CURVE ( 'NONE', #358, #2750, #4029, .T. ) ;
#1320 = EDGE_CURVE ( 'NONE', #4105, #3782, #7803, .T. ) ;
#1321 = PLANE ( 'NONE',  #7638 ) ;
#1322 = CALENDAR_DATE ( 2026, 9, 10 ) ;
#1323 = CARTESIAN_POINT ( 'NONE',  ( 0.2796912674003787513, -4.528516545235624413, 0.2179999999999999993 ) ) ;
#1324 = CARTESIAN_POINT ( 'NONE',  ( 6.000000000000001776, 0.000000000000000000, 0.1250000000000004441 ) ) ;
#1325 = ADVANCED_FACE ( 'NONE', ( #2700 ), #6531, .F. ) ;
#1326 = CC_DESIGN_PERSON_AND_ORGANIZATION_ASSIGNMENT ( #5966, #7911, ( #448 ) ) ;
#1327 = ORIENTED_EDGE ( 'NONE', *, *, #5177, .T. ) ;
#1328 = EDGE_CURVE ( 'NONE', #787, #3032, #7208, .T. ) ;
#1329 = LOCAL_TIME ( 14, 45, 32.00000000000000000, #3407 ) ;
#1330 = EDGE_CURVE ( 'NONE', #7840, #3971, #2866, .T. ) ;
#1331 = DIRECTION ( 'NONE',  ( 0.000000000000000000, 1.000000000000000000, 0.000000000000000000 ) ) ;
#1332 = ORIENTED_EDGE ( 'NONE', *, *, #6094, .T. ) ;
#1333 = VECTOR ( 'NONE', #4909, 39.37007874015748143 ) ;
#1334 = CARTESIAN_POINT ( 'NONE',  ( 1.690678803126011154, 1.376073966722298536, 0.2163527671803432417 ) ) ;
#1335 = DIRECTION ( 'NONE',  ( -0.000000000000000000, -1.000000000000000000, -0.000000000000000000 ) ) ;
#1336 = DIRECTION ( 'NONE',  ( 1.000000000000000000, 0.000000000000000000, 0.000000000000000000 ) ) ;
#1337 = CARTESIAN_POINT ( 'NONE',  ( 1.800320205903116921, 1.030513867073702183, -0.08212881570848259982 ) ) ;
#1338 = CIRCLE ( 'NONE', #5667, 8.633956053943499853 ) ;
#1339 = FACE_OUTER_BOUND ( 'NONE', #3134, .T. ) ;
#1340 = LINE ( 'NONE', #3969, #5186 ) ;
#1341 = APPROVAL_ROLE ( '' ) ;
#1342 = VERTEX_POINT ( 'NONE', #6064 ) ;
#1343 = AXIS2_PLACEMENT_3D ( 'NONE', #7003, #5151, #3923 ) ;
#1344 = DIRECTION ( 'NONE',  ( 0.000000000000000000, 0.000000000000000000, -1.000000000000000000 ) ) ;
#1345 = CARTESIAN_POINT ( 'NONE',  ( 0.7510138408322231118, -0.03124999999962550443, 0.000000000000000000 ) ) ;
#1346 = ORIENTED_EDGE ( 'NONE', *, *, #3179, .T. ) ;
#1347 = CARTESIAN_POINT ( 'NONE',  ( 1.473442587156926775, 1.198637710842282766, 0.2295096657271606944 ) ) ;
#1348 = VECTOR ( 'NONE', #4130, 39.37007874015748854 ) ;
#1349 = DIRECTION ( 'NONE',  ( -1.000000000000000000, 0.000000000000000000, 0.000000000000000000 ) ) ;
#1350 = CARTESIAN_POINT ( 'NONE',  ( -1.432604426929670938, 0.8194101287839820058, -0.1250000000000000000 ) ) ;
#1351 = CARTESIAN_POINT ( 'NONE',  ( 1.499442570351851911, 1.861459104221312000, -0.001141387575425446659 ) ) ;
#1352 = AXIS2_PLACEMENT_3D ( 'NONE', #7811, #2239, #1050 ) ;
#1353 = AXIS2_PLACEMENT_3D ( 'NONE', #3166, #2615, #5056 ) ;
#1354 = B_SPLINE_CURVE_WITH_KNOTS ( 'NONE', 3,
 ( #7297, #6835, #6721, #8054, #609, #1676, #3609, #4179, #5492, #2360, #7373, #6763 ),
 .UNSPECIFIED., .F., .F.,
 ( 4, 2, 2, 2, 2, 4 ),
 ( 8.909715784852462421E-15, 0.001906393393842450556, 0.002859590090759231689, 0.003812786787676013256, 0.005719180181509561645, 0.007625573575343111768 ),
 .UNSPECIFIED. ) ;
#1355 = CARTESIAN_POINT ( 'NONE',  ( 1.530808498934191201E-17, 0.6124999999999999334, -0.1250000000000000000 ) ) ;
#1356 = ORIENTED_EDGE ( 'NONE', *, *, #5085, .T. ) ;
#1357 = SECURITY_CLASSIFICATION ( '', '', #5632 ) ;
#1358 = TOROIDAL_SURFACE ( 'NONE', #2405, 0.2819999999999999729, 0.03200000000000000067 ) ;
#1359 = EDGE_LOOP ( 'NONE', ( #1060, #1818 ) ) ;
#1360 = DIRECTION ( 'NONE',  ( 1.000000000000000000, 0.000000000000000000, 0.000000000000000000 ) ) ;
#1361 = DIRECTION ( 'NONE',  ( -0.000000000000000000, -0.000000000000000000, -1.000000000000000000 ) ) ;
#1362 = DIRECTION ( 'NONE',  ( 1.000000000000000000, 0.000000000000000000, -0.000000000000000000 ) ) ;
#1363 = CARTESIAN_POINT ( 'NONE',  ( 0.1255000000000000282, 1.916572240665608148E-17, -0.6849999999999999423 ) ) ;
#1364 = ORIENTED_EDGE ( 'NONE', *, *, #1935, .T. ) ;
#1365 = CIRCLE ( 'NONE', #2818, 8.696493751522730520 ) ;
#1366 = EDGE_CURVE ( 'NONE', #6616, #6811, #5980, .T. ) ;
#1367 = ADVANCED_FACE ( 'NONE', ( #7294 ), #1177, .T. ) ;
#1368 = ORIENTED_EDGE ( 'NONE', *, *, #1458, .T. ) ;
#1369 = APPLICATION_CONTEXT ( 'configuration controlled 3d designs of mechanical parts and assemblies' ) ;
#1370 = DIRECTION ( 'NONE',  ( 0.6157549048526803626, -0.7879377495398139919, 0.000000000000000000 ) ) ;
#1371 = ORIENTED_EDGE ( 'NONE', *, *, #68, .T. ) ;
#1372 = CARTESIAN_POINT ( 'NONE',  ( -2.114821033088378321, 1.190739337094255168, -0.2959999999999997078 ) ) ;
#1373 = CARTESIAN_POINT ( 'NONE',  ( 0.000000000000000000, 0.6250000000000000000, 0.000000000000000000 ) ) ;
#1374 = EDGE_CURVE ( 'NONE', #6326, #2455, #8050, .T. ) ;
#1375 = LINE ( 'NONE', #148, #2506 ) ;
#1376 = DIRECTION ( 'NONE',  ( 0.000000000000000000, 0.000000000000000000, 1.000000000000000000 ) ) ;
#1377 = CIRCLE ( 'NONE', #3614, 0.1150000000000000050 ) ;
#1378 = EDGE_LOOP ( 'NONE', ( #7311, #2409, #7432, #799 ) ) ;
#1379 = AXIS2_PLACEMENT_3D ( 'NONE', #1672, #2897, #3479 ) ;
#1380 = VERTEX_POINT ( 'NONE', #2286 ) ;
#1381 = CARTESIAN_POINT ( 'NONE',  ( 1.800774122434213975, 1.436334721442235507, 0.1268433716242569342 ) ) ;
#1382 = LINE ( 'NONE', #1927, #3094 ) ;
#1383 = VECTOR ( 'NONE', #987, 39.37007874015748143 ) ;
#1384 = PERSON_AND_ORGANIZATION ( #4735, #6190 ) ;
#1385 = ORIENTED_EDGE ( 'NONE', *, *, #3138, .T. ) ;
#1386 = DIRECTION ( 'NONE',  ( 0.9891211992429681521, 0.000000000000000000, 0.1471028660772870089 ) ) ;
#1387 = ORIENTED_EDGE ( 'NONE', *, *, #1039, .F. ) ;
#1388 = AXIS2_PLACEMENT_3D ( 'NONE', #2599, #5650, #5106 ) ;
#1389 = CARTESIAN_POINT ( 'NONE',  ( 3.672767723898985537, -8.314396374632453401, 0.1250000000000000000 ) ) ;
#1390 = CIRCLE ( 'NONE', #5983, 0.1250000000000000000 ) ;
#1391 = ORIENTED_EDGE ( 'NONE', *, *, #6543, .F. ) ;
#1392 = AXIS2_PLACEMENT_3D ( 'NONE', #5240, #5894, #7202 ) ;
#1393 = CARTESIAN_POINT ( 'NONE',  ( 0.000000000000000000, 0.000000000000000000, -0.1487499999999999933 ) ) ;
#1394 = CARTESIAN_POINT ( 'NONE',  ( -2.290684594132797791, -0.9654407352564655653, 0.6477670380269010542 ) ) ;
#1395 = DIRECTION ( 'NONE',  ( 0.000000000000000000, 0.000000000000000000, -1.000000000000000000 ) ) ;
#1396 = CONTEXT_DEPENDENT_SHAPE_REPRESENTATION ( #1221, #5919 ) ;
#1397 = CARTESIAN_POINT ( 'NONE',  ( 1.877300571085743108, 1.420647526259452897, -0.06641314542006129806 ) ) ;
#1398 = DIRECTION ( 'NONE',  ( -0.9987955914953423608, -0.04906492035527430795, -0.000000000000000000 ) ) ;
#1399 = CIRCLE ( 'NONE', #5993, 0.06250000000000000000 ) ;
#1400 = CIRCLE ( 'NONE', #4293, 0.1799999999999999933 ) ;
#1401 = ORIENTED_EDGE ( 'NONE', *, *, #1289, .F. ) ;
#1402 = EDGE_LOOP ( 'NONE', ( #4754, #2737, #7775, #2210 ) ) ;
#1403 = DIRECTION ( 'NONE',  ( 0.7879377495398138809, 0.6157549048526802515, 0.000000000000000000 ) ) ;
#1404 = PERSON_AND_ORGANIZATION_ROLE ( 'creator' ) ;
#1405 = CARTESIAN_POINT ( 'NONE',  ( 1.651097472914581088, 1.707757380030753280, -0.06087441991423112042 ) ) ;
#1406 = DIRECTION ( 'NONE',  ( 0.6157549048526803626, -0.7879377495398141029, 0.000000000000000000 ) ) ;
#1407 = ORIENTED_EDGE ( 'NONE', *, *, #3887, .F. ) ;
#1408 =( BOUNDED_CURVE ( )  B_SPLINE_CURVE ( 3, ( #454, #5500, #1192, #5536 ),
 .UNSPECIFIED., .F., .T. ) 
 B_SPLINE_CURVE_WITH_KNOTS ( ( 4, 4 ),
 ( 1.570796326794900555, 3.141592653589790896 ),
 .UNSPECIFIED. ) 
 CURVE ( )  GEOMETRIC_REPRESENTATION_ITEM ( )  RATIONAL_B_SPLINE_CURVE ( ( 1.000000000000000000, 0.8047378541243663808, 0.8047378541243663808, 1.000000000000000000 ) ) 
 REPRESENTATION_ITEM ( '' )  );
#1409 = ORIENTED_EDGE ( 'NONE', *, *, #1835, .T. ) ;
#1410 = ORIENTED_EDGE ( 'NONE', *, *, #6214, .F. ) ;
#1411 = ORIENTED_EDGE ( 'NONE', *, *, #90, .T. ) ;
#1412 = EDGE_LOOP ( 'NONE', ( #4053, #7854, #6735, #2100 ) ) ;
#1413 = CARTESIAN_POINT ( 'NONE',  ( -1.067641779222573639, 0.6107141540073631747, -0.1250000000000000000 ) ) ;
#1414 = ORIENTED_EDGE ( 'NONE', *, *, #8090, .T. ) ;
#1415 = DIRECTION ( 'NONE',  ( 0.7540216022612858948, -0.6568496200222110337, 0.000000000000000000 ) ) ;
#1416 = CARTESIAN_POINT ( 'NONE',  ( 0.06250000000000000000, 7.654042494670957545E-18, 0.09374999999999998612 ) ) ;
#1417 = ADVANCED_FACE ( 'NONE', ( #6024 ), #4144, .T. ) ;
#1418 = LINE ( 'NONE', #3472, #6836 ) ;
#1419 = CARTESIAN_POINT ( 'NONE',  ( 0.2386870781737283065, -0.03125000000000000000, 0.000000000000000000 ) ) ;
#1420 = ADVANCED_FACE ( 'NONE', ( #8012 ), #5570, .F. ) ;
#1421 = CARTESIAN_POINT ( 'NONE',  ( 1.496141785815785941, 1.858879618380945509, -0.01305819514303249197 ) ) ;
#1422 = DIRECTION ( 'NONE',  ( -0.7879377495398142139, -0.6157549048526800295, 0.000000000000000000 ) ) ;
#1423 = APPROVAL_DATE_TIME ( #6529, #2994 ) ;
#1424 = EDGE_CURVE ( 'NONE', #1929, #255, #6112, .T. ) ;
#1425 = DIRECTION ( 'NONE',  ( -0.000000000000000000, -1.000000000000000000, -0.000000000000000000 ) ) ;
#1426 = CARTESIAN_POINT ( 'NONE',  ( 1.294204688232935219, 1.088727781300392827, -0.1026931866138307559 ) ) ;
#1427 = CARTESIAN_POINT ( 'NONE',  ( -0.03125000000000000000, -0.03125000000000000000, 0.000000000000000000 ) ) ;
#1428 = VERTEX_POINT ( 'NONE', #5449 ) ;
#1429 = ADVANCED_FACE ( 'NONE', ( #525 ), #4302, .T. ) ;
#1430 = DIRECTION ( 'NONE',  ( -3.552713678800500929E-15, 0.000000000000000000, 1.000000000000000000 ) ) ;
#1431 = CC_DESIGN_PERSON_AND_ORGANIZATION_ASSIGNMENT ( #6821, #2511, ( #5651 ) ) ;
#1432 = EDGE_CURVE ( 'NONE', #3897, #7385, #558, .T. ) ;
#1433 = DIRECTION ( 'NONE',  ( -1.000000000000000000, -0.000000000000000000, -0.000000000000000000 ) ) ;
#1434 = CARTESIAN_POINT ( 'NONE',  ( 1.408343819019455843E-17, 0.03124999999999997571, 0.1150000000000000050 ) ) ;
#1435 = PERSON_AND_ORGANIZATION_ROLE ( 'creator' ) ;
#1436 = ORIENTED_EDGE ( 'NONE', *, *, #679, .F. ) ;
#1437 = DATE_TIME_ROLE ( 'classification_date' ) ;
#1438 = CARTESIAN_POINT ( 'NONE',  ( 0.000000000000000000, 0.000000000000000000, 0.1250000000000000000 ) ) ;
#1439 = PLANE ( 'NONE',  #1601 ) ;
#1440 = EDGE_CURVE ( 'NONE', #2815, #3298, #3620, .T. ) ;
#1441 = ORIENTED_EDGE ( 'NONE', *, *, #7537, .F. ) ;
#1442 = CARTESIAN_POINT ( 'NONE',  ( -3.165020334763531729, -1.163753072338894023, 0.1250000000000000000 ) ) ;
#1443 = DATE_AND_TIME ( #1322, #5792 ) ;
#1444 = DIRECTION ( 'NONE',  ( 0.000000000000000000, -1.000000000000000000, 0.000000000000000000 ) ) ;
#1445 = DIRECTION ( 'NONE',  ( 0.000000000000000000, 0.000000000000000000, -1.000000000000000000 ) ) ;
#1446 = ORIENTED_EDGE ( 'NONE', *, *, #5030, .F. ) ;
#1447 = ORIENTED_EDGE ( 'NONE', *, *, #5093, .T. ) ;
#1448 = VERTEX_POINT ( 'NONE', #7413 ) ;
#1449 = VERTEX_POINT ( 'NONE', #1145 ) ;
#1450 = LOCAL_TIME ( 14, 45, 32.00000000000000000, #7377 ) ;
#1451 = PLANE ( 'NONE',  #4502 ) ;
#1452 = ORIENTED_EDGE ( 'NONE', *, *, #2791, .T. ) ;
#1453 = CARTESIAN_POINT ( 'NONE',  ( 1.719796567415322386, 1.364484731518883498, 0.1975831474265880849 ) ) ;
#1454 =( BOUNDED_SURFACE ( )  B_SPLINE_SURFACE ( 3, 2, ( 
 ( #3413, #996, #5300 ),
 ( #6605, #6567, #7857 ),
 ( #5413, #2870, #3564 ),
 ( #951, #1597, #7257 ),
 ( #5997, #2181, #4680 ),
 ( #6646, #5952, #2952 ) ),
 .UNSPECIFIED., .F., .F., .T. ) 
 B_SPLINE_SURFACE_WITH_KNOTS ( ( 4, 2, 4 ),
 ( 3, 3 ),
 ( -1.528269698292117340E-14, 0.0008095007283496732150, 0.001619001456714629127 ),
 ( 0.000000000000000000, 1.000000000000000000 ),
 .UNSPECIFIED. ) 
 GEOMETRIC_REPRESENTATION_ITEM ( )  RATIONAL_B_SPLINE_SURFACE ( (
 ( 1.000000000000000000, 0.7071067811870255237, 1.000000000000000000),
 ( 1.000000000000000000, 0.7102386623011891498, 1.000000000000000000),
 ( 1.000000000000000000, 0.7133082652150437575, 1.000000000000000000),
 ( 1.000000000000000000, 0.7193245599450390770, 1.000000000000000000),
 ( 1.000000000000000000, 0.7222974223247246028, 1.000000000000000000),
 ( 1.000000000000000000, 0.7250243206839943610, 1.000000000000000000) ) ) 
 REPRESENTATION_ITEM ( '' )  SURFACE ( )  );
#1455 = CARTESIAN_POINT ( 'NONE',  ( 3.221700243049672174, 0.8684880333666047392, -0.1849999999999999978 ) ) ;
#1456 = DIRECTION ( 'NONE',  ( -0.000000000000000000, -0.000000000000000000, 1.000000000000000000 ) ) ;
#1457 = CARTESIAN_POINT ( 'NONE',  ( -1.855136387357835481, 0.9645206712600612464, 0.1339999999999995361 ) ) ;
#1458 = EDGE_CURVE ( 'NONE', #810, #5561, #7937, .T. ) ;
#1459 = CIRCLE ( 'NONE', #6055, 0.2112499999999999933 ) ;
#1460 = AXIS2_PLACEMENT_3D ( 'NONE', #1938, #166, #6899 ) ;
#1461 = CARTESIAN_POINT ( 'NONE',  ( 1.762871904346776653, 1.395378910334173828, 0.1649876832364386703 ) ) ;
#1462 = APPROVAL_PERSON_ORGANIZATION ( #737, #1185, #6886 ) ;
#1463 = DATE_TIME_ROLE ( 'classification_date' ) ;
#1464 = LINE ( 'NONE', #5210, #851 ) ;
#1465 = CYLINDRICAL_SURFACE ( 'NONE', #625, 0.5000000000000279776 ) ;
#1466 = CARTESIAN_POINT ( 'NONE',  ( 0.000000000000000000, 0.000000000000000000, 0.000000000000000000 ) ) ;
#1467 = ORIENTED_EDGE ( 'NONE', *, *, #7639, .T. ) ;
#1468 = AXIS2_PLACEMENT_3D ( 'NONE', #6681, #6164, #2415 ) ;
#1469 = CARTESIAN_POINT ( 'NONE',  ( 1.258616367985684104, -0.02482036785324303815, -0.1250000000000000000 ) ) ;
#1470 = APPROVAL_PERSON_ORGANIZATION ( #6438, #1278, #5826 ) ;
#1471 = SECURITY_CLASSIFICATION ( '', '', #4525 ) ;
#1472 = EDGE_CURVE ( 'NONE', #3734, #5716, #3875, .T. ) ;
#1473 = CARTESIAN_POINT ( 'NONE',  ( 1.251356423955005015, 1.643685595130192745, 0.2500000000000000000 ) ) ;
#1474 = CARTESIAN_POINT ( 'NONE',  ( 1.733157827470031220, 1.373632878362992527, 0.1887011865795288901 ) ) ;
#1475 = COORDINATED_UNIVERSAL_TIME_OFFSET ( 0, 0, .AHEAD. ) ;
#1476 = VERTEX_POINT ( 'NONE', #1711 ) ;
#1477 = CC_DESIGN_PERSON_AND_ORGANIZATION_ASSIGNMENT ( #7348, #6086, ( #1105 ) ) ;
#1478 = DIRECTION ( 'NONE',  ( 0.000000000000000000, 0.000000000000000000, 1.000000000000000000 ) ) ;
#1479 = EDGE_CURVE ( 'NONE', #789, #4769, #7158, .T. ) ;
#1480 = CARTESIAN_POINT ( 'NONE',  ( 1.258671604940865274, -0.02501003737716508274, 5.393636709996481038 ) ) ;
#1481 = EDGE_CURVE ( 'NONE', #3319, #2575, #1026, .T. ) ;
#1482 = AXIS2_PLACEMENT_3D ( 'NONE', #7574, #3810, #72 ) ;
#1483 = ORIENTED_EDGE ( 'NONE', *, *, #5349, .T. ) ;
#1484 = ORIENTED_EDGE ( 'NONE', *, *, #6793, .T. ) ;
#1485 = CIRCLE ( 'NONE', #6215, 8.573908398499121120 ) ;
#1486 =( LENGTH_UNIT ( ) NAMED_UNIT ( * ) SI_UNIT ( $, .METRE. ) );
#1487 = CARTESIAN_POINT ( 'NONE',  ( 3.672798492683009286, -8.252032378159654513, 0.1850000000000003586 ) ) ;
#1488 = VECTOR ( 'NONE', #6021, 39.37007874015748143 ) ;
#1489 = DIRECTION ( 'NONE',  ( -0.000000000000000000, -1.000000000000000000, -0.000000000000000000 ) ) ;
#1490 = DATE_AND_TIME ( #5270, #4354 ) ;
#1491 = DIRECTION ( 'NONE',  ( 0.6568496200222107007, 0.7540216022612862279, -0.000000000000000000 ) ) ;
#1492 = CARTESIAN_POINT ( 'NONE',  ( 0.6690408158126811555, -0.04637372973215107830, 0.07449999999999999678 ) ) ;
#1493 = ORIENTED_EDGE ( 'NONE', *, *, #2362, .T. ) ;
#1494 = ORIENTED_EDGE ( 'NONE', *, *, #2362, .F. ) ;
#1495 = EDGE_LOOP ( 'NONE', ( #3915, #4320, #4632, #7245 ) ) ;
#1496 = CC_DESIGN_SECURITY_CLASSIFICATION ( #51, ( #8098 ) ) ;
#1497 = AXIS2_PLACEMENT_3D ( 'NONE', #1580, #389, #5891 ) ;
#1498 = ORIENTED_EDGE ( 'NONE', *, *, #1481, .F. ) ;
#1499 = ORIENTED_EDGE ( 'NONE', *, *, #6903, .F. ) ;
#1500 = CARTESIAN_POINT ( 'NONE',  ( 1.780616048947831098, 1.055727875058976251, -0.08212881570848259982 ) ) ;
#1501 = VERTEX_POINT ( 'NONE', #6111 ) ;
#1502 = CARTESIAN_POINT ( 'NONE',  ( 1.704817408831214021, 1.367523911545252879, 0.2140310551078935808 ) ) ;
#1503 = CARTESIAN_POINT ( 'NONE',  ( -1.763177565995707630, 1.070083551578369763, -0.08100000000000007194 ) ) ;
#1504 = AXIS2_PLACEMENT_3D ( 'NONE', #3177, #1406, #6372 ) ;
#1505 = CIRCLE ( 'NONE', #7907, 0.01652128394798136474 ) ;
#1506 = CARTESIAN_POINT ( 'NONE',  ( 0.000000000000000000, 0.000000000000000000, -0.6849999999999999423 ) ) ;
#1507 = DIRECTION ( 'NONE',  ( -0.000000000000000000, -0.000000000000000000, 1.000000000000000000 ) ) ;
#1508 = AXIS2_PLACEMENT_3D ( 'NONE', #1977, #4568, #5725 ) ;
#1509 = VECTOR ( 'NONE', #2535, 39.37007874015748143 ) ;
#1510 = CARTESIAN_POINT ( 'NONE',  ( 1.440344085072671199, 1.815275021530317279, 0.1087460313510809767 ) ) ;
#1511 = CARTESIAN_POINT ( 'NONE',  ( 1.535041889452112285, 1.849375524390286740, -0.03191141767805402707 ) ) ;
#1512 = APPROVAL_ROLE ( '' ) ;
#1513 = CARTESIAN_POINT ( 'NONE',  ( -0.03125000000000000000, 0.03125000000000000000, -0.1204106507132265275 ) ) ;
#1514 = CARTESIAN_POINT ( 'NONE',  ( 0.2796912674001651444, -4.528516545235133250, 0.3125000000000000000 ) ) ;
#1515 = VECTOR ( 'NONE', #5115, 39.37007874015748143 ) ;
#1516 = ORIENTED_EDGE ( 'NONE', *, *, #1879, .F. ) ;
#1517 = CARTESIAN_POINT ( 'NONE',  ( -0.1249999999999999445, -0.03125000000000000000, 0.06250000000000000000 ) ) ;
#1518 = VECTOR ( 'NONE', #1059, 39.37007874015748143 ) ;
#1519 = DIRECTION ( 'NONE',  ( 0.6157549048526804736, -0.7879377495398138809, -0.000000000000000000 ) ) ;
#1520 = DIRECTION ( 'NONE',  ( 0.000000000000000000, 0.000000000000000000, 1.000000000000000000 ) ) ;
#1521 = PERSON_AND_ORGANIZATION ( #4735, #6190 ) ;
#1522 = EDGE_LOOP ( 'NONE', ( #335, #7864, #5917 ) ) ;
#1523 = ORIENTED_EDGE ( 'NONE', *, *, #7550, .T. ) ;
#1524 = CIRCLE ( 'NONE', #6116, 0.3024878104020024550 ) ;
#1525 = AXIS2_PLACEMENT_3D ( 'NONE', #6813, #3742, #4316 ) ;
#1526 = PLANE ( 'NONE',  #6757 ) ;
#1527 = ADVANCED_FACE ( 'NONE', ( #3523 ), #398, .F. ) ;
#1528 = CARTESIAN_POINT ( 'NONE',  ( 1.473750031596730237, 1.199377247893690601, 0.2292416509145525638 ) ) ;
#1529 = AXIS2_PLACEMENT_3D ( 'NONE', #4947, #7965, #3640 ) ;
#1530 = ORIENTED_EDGE ( 'NONE', *, *, #7928, .F. ) ;
#1531 = EDGE_CURVE ( 'NONE', #1125, #2232, #6707, .T. ) ;
#1532 = DIRECTION ( 'NONE',  ( 0.000000000000000000, 0.000000000000000000, -1.000000000000000000 ) ) ;
#1533 = FACE_OUTER_BOUND ( 'NONE', #3079, .T. ) ;
#1534 = COORDINATED_UNIVERSAL_TIME_OFFSET ( 0, 0, .AHEAD. ) ;
#1535 = DIRECTION ( 'NONE',  ( 0.000000000000000000, 0.000000000000000000, 1.000000000000000000 ) ) ;
#1536 = EDGE_CURVE ( 'NONE', #1856, #409, #1920, .T. ) ;
#1537 = EDGE_CURVE ( 'NONE', #1539, #761, #30, .T. ) ;
#1538 = EDGE_CURVE ( 'NONE', #5954, #787, #3561, .T. ) ;
#1539 = VERTEX_POINT ( 'NONE', #3114 ) ;
#1540 = VECTOR ( 'NONE', #4188, 39.37007874015748143 ) ;
#1541 = APPLICATION_CONTEXT ( 'configuration controlled 3d designs of mechanical parts and assemblies' ) ;
#1542 = ORIENTED_EDGE ( 'NONE', *, *, #7527, .F. ) ;
#1543 = AXIS2_PLACEMENT_3D ( 'NONE', #4921, #4270, #6119 ) ;
#1544 = VERTEX_POINT ( 'NONE', #5616 ) ;
#1545 = CC_DESIGN_DATE_AND_TIME_ASSIGNMENT ( #2650, #1463, ( #5523 ) ) ;
#1546 = EDGE_CURVE ( 'NONE', #4226, #7842, #7326, .T. ) ;
#1547 = ORIENTED_EDGE ( 'NONE', *, *, #1690, .F. ) ;
#1548 = DIRECTION ( 'NONE',  ( 1.000000000000000000, 0.000000000000000000, 0.000000000000000000 ) ) ;
#1549 = DESIGN_CONTEXT ( 'detailed design', #6566, 'design' ) ;
#1550 = ORIENTED_EDGE ( 'NONE', *, *, #170, .F. ) ;
#1551 = LINE ( 'NONE', #2976, #2532 ) ;
#1552 = CYLINDRICAL_SURFACE ( 'NONE', #3234, 0.03124999999999985428 ) ;
#1553 = FACE_OUTER_BOUND ( 'NONE', #960, .T. ) ;
#1554 = DIRECTION ( 'NONE',  ( -1.000000000000000000, 0.000000000000000000, -0.000000000000000000 ) ) ;
#1555 = VERTEX_POINT ( 'NONE', #6832 ) ;
#1556 = CARTESIAN_POINT ( 'NONE',  ( 1.268245620182552935, 1.680784100216294652, 0.2179999999999998883 ) ) ;
#1557 = CARTESIAN_POINT ( 'NONE',  ( 3.659299226295303686, -8.245510427152350275, 5.393636709996481038 ) ) ;
#1558 = DIRECTION ( 'NONE',  ( 1.000000000000000000, 0.000000000000000000, 0.000000000000000000 ) ) ;
#1559 = VERTEX_POINT ( 'NONE', #3189 ) ;
#1560 = DIRECTION ( 'NONE',  ( 0.000000000000000000, 0.000000000000000000, -1.000000000000000000 ) ) ;
#1561 = LINE ( 'NONE', #3446, #5690 ) ;
#1562 = CARTESIAN_POINT ( 'NONE',  ( 1.975095093049261896, 1.207708695074841909, -0.1039999999999998703 ) ) ;
#1563 = PERSON_AND_ORGANIZATION_ROLE ( 'design_supplier' ) ;
#1564 = ORIENTED_EDGE ( 'NONE', *, *, #7592, .T. ) ;
#1565 = DIRECTION ( 'NONE',  ( 0.000000000000000000, 0.000000000000000000, 1.000000000000000000 ) ) ;
#1566 = CARTESIAN_POINT ( 'NONE',  ( 1.449725606736619543, 1.190739840090658364, 0.2500000000000000000 ) ) ;
#1567 = ORIENTED_EDGE ( 'NONE', *, *, #68, .F. ) ;
#1568 = ORIENTED_EDGE ( 'NONE', *, *, #2612, .T. ) ;
#1569 = EDGE_CURVE ( 'NONE', #695, #2111, #2627, .T. ) ;
#1570 = ORIENTED_EDGE ( 'NONE', *, *, #6143, .F. ) ;
#1571 = CARTESIAN_POINT ( 'NONE',  ( 0.000000000000000000, 1.081250000000000044, 0.000000000000000000 ) ) ;
#1572 = LINE ( 'NONE', #5881, #224 ) ;
#1573 = APPROVAL_ROLE ( '' ) ;
#1574 = CARTESIAN_POINT ( 'NONE',  ( -6.420602001755994159, -1.404684638105634820, -0.05999999999999999778 ) ) ;
#1575 = VERTEX_POINT ( 'NONE', #4990 ) ;
#1576 = VERTEX_POINT ( 'NONE', #6232 ) ;
#1577 = EDGE_CURVE ( 'NONE', #4309, #5382, #5768, .T. ) ;
#1578 = EDGE_CURVE ( 'NONE', #3032, #5193, #3305, .T. ) ;
#1579 = EDGE_CURVE ( 'NONE', #1342, #3595, #4382, .T. ) ;
#1580 = CARTESIAN_POINT ( 'NONE',  ( 0.1255000000000000282, 1.536931732929928570E-17, -0.6219999999999999973 ) ) ;
#1581 = EDGE_CURVE ( 'NONE', #684, #7184, #2119, .T. ) ;
#1582 = DIRECTION ( 'NONE',  ( 0.000000000000000000, -0.000000000000000000, 1.000000000000000000 ) ) ;
#1583 = FACE_OUTER_BOUND ( 'NONE', #7438, .T. ) ;
#1584 = CC_DESIGN_DATE_AND_TIME_ASSIGNMENT ( #5064, #7719, ( #3498 ) ) ;
#1585 = DIRECTION ( 'NONE',  ( -0.000000000000000000, 1.000000000000000000, -0.000000000000000000 ) ) ;
#1586 = EDGE_CURVE ( 'NONE', #6271, #5004, #1987, .T. ) ;
#1587 = DIRECTION ( 'NONE',  ( -0.000000000000000000, -1.000000000000000000, -0.000000000000000000 ) ) ;
#1588 = CARTESIAN_POINT ( 'NONE',  ( 1.800320205903116921, 1.030513867073702183, -0.08212881570848259982 ) ) ;
#1589 = DIRECTION ( 'NONE',  ( 0.000000000000000000, 0.000000000000000000, 1.000000000000000000 ) ) ;
#1590 = CARTESIAN_POINT ( 'NONE',  ( 0.3265803234075882466, -0.3651282914590817663, 0.004338029470932578714 ) ) ;
#1591 = ORIENTED_EDGE ( 'NONE', *, *, #3873, .T. ) ;
#1592 = DIRECTION ( 'NONE',  ( -0.000000000000000000, -0.000000000000000000, -1.000000000000000000 ) ) ;
#1593 = ADVANCED_FACE ( 'NONE', ( #5033 ), #4429, .T. ) ;
#1594 = AXIS2_PLACEMENT_3D ( 'NONE', #1318, #4481, #672 ) ;
#1595 = CC_DESIGN_SECURITY_CLASSIFICATION ( #7867, ( #4603 ) ) ;
#1596 = LINE ( 'NONE', #6118, #720 ) ;
#1597 = CARTESIAN_POINT ( 'NONE',  ( 1.515492104094517067, 1.874001439105450473, -0.01551275274473707180 ) ) ;
#1598 = COORDINATED_UNIVERSAL_TIME_OFFSET ( 0, 0, .AHEAD. ) ;
#1599 = ORIENTED_EDGE ( 'NONE', *, *, #4190, .F. ) ;
#1600 = ORIENTED_EDGE ( 'NONE', *, *, #1472, .T. ) ;
#1601 = AXIS2_PLACEMENT_3D ( 'NONE', #212, #132, #3058 ) ;
#1602 = CARTESIAN_POINT ( 'NONE',  ( 1.491230041056485378, 1.855041204840421232, -0.04518674047500752938 ) ) ;
#1603 = APPROVAL_PERSON_ORGANIZATION ( #641, #4591, #3102 ) ;
#1604 = CARTESIAN_POINT ( 'NONE',  ( 6.213241126991890795, 0.5142750483228147873, 5.393636709996481038 ) ) ;
#1605 = EDGE_LOOP ( 'NONE', ( #7908, #6833, #2955, #7046 ) ) ;
#1606 = AXIS2_PLACEMENT_3D ( 'NONE', #7055, #662, #3162 ) ;
#1607 = VERTEX_POINT ( 'NONE', #1837 ) ;
#1608 = ORIENTED_EDGE ( 'NONE', *, *, #4738, .F. ) ;
#1609 = CARTESIAN_POINT ( 'NONE',  ( 1.868427082838399311, 1.436511782911442880, -0.04381998756813935969 ) ) ;
#1610 = DIRECTION ( 'NONE',  ( 0.000000000000000000, 0.000000000000000000, 1.000000000000000000 ) ) ;
#1611 = CALENDAR_DATE ( 2026, 9, 10 ) ;
#1612 = DIRECTION ( 'NONE',  ( -0.000000000000000000, -1.000000000000000000, -0.000000000000000000 ) ) ;
#1613 = AXIS2_PLACEMENT_3D ( 'NONE', #286, #2788, #2248 ) ;
#1614 = VERTEX_POINT ( 'NONE', #3845 ) ;
#1615 = ORIENTED_EDGE ( 'NONE', *, *, #7985, .F. ) ;
#1616 = ORIENTED_EDGE ( 'NONE', *, *, #5131, .T. ) ;
#1617 = ORIENTED_EDGE ( 'NONE', *, *, #6005, .T. ) ;
#1618 = CIRCLE ( 'NONE', #833, 0.3750000000000000555 ) ;
#1619 = DIRECTION ( 'NONE',  ( 1.000000000000000000, -8.943549979258001330E-15, 0.000000000000000000 ) ) ;
#1620 = DIRECTION ( 'NONE',  ( -1.000000000000000000, 0.000000000000000000, 0.000000000000000000 ) ) ;
#1621 = VERTEX_POINT ( 'NONE', #1955 ) ;
#1622 = ADVANCED_FACE ( 'NONE', ( #6957 ), #6349, .F. ) ;
#1623 = CARTESIAN_POINT ( 'NONE',  ( 1.460659702294222928, 1.192157774404229764, 0.2321080476372760493 ) ) ;
#1624 = EDGE_CURVE ( 'NONE', #7141, #7062, #1375, .T. ) ;
#1625 = DIRECTION ( 'NONE',  ( 0.000000000000000000, 0.000000000000000000, 1.000000000000000000 ) ) ;
#1626 = LOCAL_TIME ( 14, 45, 32.00000000000000000, #3422 ) ;
#1627 = AXIS2_PLACEMENT_3D ( 'NONE', #7809, #4012, #4662 ) ;
#1628 = FACE_BOUND ( 'NONE', #4643, .T. ) ;
#1629 = ADVANCED_FACE ( 'NONE', ( #1992 ), #4498, .T. ) ;
#1630 = CARTESIAN_POINT ( 'NONE',  ( 1.535339692041459925, 1.850303721083318420, -0.01584850669601754747 ) ) ;
#1631 = LINE ( 'NONE', #916, #2434 ) ;
#1632 = ORIENTED_EDGE ( 'NONE', *, *, #4203, .T. ) ;
#1633 = CARTESIAN_POINT ( 'NONE',  ( -2.022862211726251136, 1.296302217412564017, -0.2959999999999997078 ) ) ;
#1634 = AXIS2_PLACEMENT_3D ( 'NONE', #6302, #3951, #104 ) ;
#1635 = AXIS2_PLACEMENT_3D ( 'NONE', #7302, #4878, #1760 ) ;
#1636 = CARTESIAN_POINT ( 'NONE',  ( -1.202422216336444860, -0.2106116882872802742, 0.01209463403148830843 ) ) ;
#1637 = APPLICATION_CONTEXT ( 'configuration controlled 3d designs of mechanical parts and assemblies' ) ;
#1638 = CARTESIAN_POINT ( 'NONE',  ( 3.566133519791359507, 0.3212125039962153705, 0.000000000000000000 ) ) ;
#1639 = CALENDAR_DATE ( 2026, 9, 10 ) ;
#1640 = ORIENTED_EDGE ( 'NONE', *, *, #329, .F. ) ;
#1641 = LINE ( 'NONE', #1067, #4944 ) ;
#1642 = CARTESIAN_POINT ( 'NONE',  ( 1.640223930642276118, 1.235377681956740803, -0.1039999999999998703 ) ) ;
#1643 = CARTESIAN_POINT ( 'NONE',  ( 0.000000000000000000, 0.000000000000000000, 0.06300000000000000044 ) ) ;
#1644 = AXIS2_PLACEMENT_3D ( 'NONE', #7216, #7715, #5955 ) ;
#1645 = VERTEX_POINT ( 'NONE', #2687 ) ;
#1646 = VECTOR ( 'NONE', #3895, 39.37007874015748143 ) ;
#1647 = AXIS2_PLACEMENT_3D ( 'NONE', #5744, #5211, #1386 ) ;
#1648 =( CONVERSION_BASED_UNIT ( 'INCH', #345 ) LENGTH_UNIT ( ) NAMED_UNIT ( #3120 ) );
#1649 = VERTEX_POINT ( 'NONE', #3308 ) ;
#1650 = CARTESIAN_POINT ( 'NONE',  ( -1.052129263295328521, 0.6378420796487936917, 0.09374999999999998612 ) ) ;
#1651 = SPHERICAL_SURFACE ( 'NONE', #2854, 0.01652128394798136474 ) ;
#1652 = CALENDAR_DATE ( 2026, 9, 10 ) ;
#1653 = AXIS2_PLACEMENT_3D ( 'NONE', #284, #2214, #4710 ) ;
#1654 = AXIS2_PLACEMENT_3D ( 'NONE', #1503, #2115, #2768 ) ;
#1655 = AXIS2_PLACEMENT_3D ( 'NONE', #7962, #5432, #6219 ) ;
#1656 = LINE ( 'NONE', #7274, #1754 ) ;
#1658 = FACE_OUTER_BOUND ( 'NONE', #3878, .T. ) ;
#1657 = AXIS2_PLACEMENT_3D ( 'NONE', #1267, #2456, #1930 ) ;
#1659 = APPROVAL_DATE_TIME ( #5157, #89 ) ;
#1660 = CARTESIAN_POINT ( 'NONE',  ( 0.000000000000000000, 0.7500000000000001110, 0.000000000000000000 ) ) ;
#1661 = CIRCLE ( 'NONE', #6375, 0.1250000000000000000 ) ;
#1662 = ORIENTED_EDGE ( 'NONE', *, *, #82, .T. ) ;
#1663 = EDGE_LOOP ( 'NONE', ( #31, #2092, #1356, #4244 ) ) ;
#1664 = DIRECTION ( 'NONE',  ( -0.000000000000000000, -1.000000000000000000, -0.000000000000000000 ) ) ;
#1665 = AXIS2_PLACEMENT_3D ( 'NONE', #156, #83, #3931 ) ;
#1666 = AXIS2_PLACEMENT_3D ( 'NONE', #2253, #4759, #2905 ) ;
#1667 = ORIENTED_EDGE ( 'NONE', *, *, #2926, .F. ) ;
#1668 = EDGE_CURVE ( 'NONE', #3019, #7983, #4666, .T. ) ;
#1669 = ADVANCED_FACE ( 'NONE', ( #7649 ), #4018, .T. ) ;
#1670 = ORIENTED_EDGE ( 'NONE', *, *, #2725, .T. ) ;
#1671 = CARTESIAN_POINT ( 'NONE',  ( -1.040997396242601791, -0.7528336330030669377, 0.03199999999999999373 ) ) ;
#1672 = CARTESIAN_POINT ( 'NONE',  ( -0.9280291358773672394, 0.8548654847802351631, -0.09374999999999998612 ) ) ;
#1673 = EDGE_CURVE ( 'NONE', #6544, #6217, #4609, .T. ) ;
#1674 = DIRECTION ( 'NONE',  ( -0.000000000000000000, -0.000000000000000000, -1.000000000000000000 ) ) ;
#1675 = ORIENTED_EDGE ( 'NONE', *, *, #3188, .T. ) ;
#1676 = CARTESIAN_POINT ( 'NONE',  ( 1.620624198909131453, 1.220060950454640913, 0.1980431631100827705 ) ) ;
#1677 =( BOUNDED_CURVE ( )  B_SPLINE_CURVE ( 3, ( #6560, #2212, #7934, #3438 ),
 .UNSPECIFIED., .F., .T. ) 
 B_SPLINE_CURVE_WITH_KNOTS ( ( 4, 4 ),
 ( 2.185478394931412941E-15, 1.570796326794896558 ),
 .UNSPECIFIED. ) 
 CURVE ( )  GEOMETRIC_REPRESENTATION_ITEM ( )  RATIONAL_B_SPLINE_CURVE ( ( 1.000000000000000000, 0.8047378541243654926, 0.8047378541243654926, 1.000000000000000000 ) ) 
 REPRESENTATION_ITEM ( '' )  );
#1678 = ADVANCED_FACE ( 'NONE', ( #189 ), #5201, .T. ) ;
#1679 = B_SPLINE_CURVE_WITH_KNOTS ( 'NONE', 3,
 ( #4396, #5045, #6888, #3159, #5662, #40, #7737, #862, #1426, #6430, #6318, #1962, #739, #7658 ),
 .UNSPECIFIED., .F., .F.,
 ( 4, 2, 2, 2, 2, 2, 4 ),
 ( 0.0003647048759916438976, 0.001831661078496667119, 0.003298617281001690448, 0.004032095382254203414, 0.004765573483506716813, 0.005499051584759229346, 0.006232529686011742745 ),
 .UNSPECIFIED. ) ;
#1680 = EDGE_CURVE ( 'NONE', #4572, #6392, #1418, .T. ) ;
#1681 = CARTESIAN_POINT ( 'NONE',  ( 0.1250000000000000278, -0.03125000000000000000, 0.06250000000000000000 ) ) ;
#1682 = CARTESIAN_POINT ( 'NONE',  ( 1.398758944919299640, 1.188821657285198841, 0.2500000000000000000 ) ) ;
#1683 = COORDINATED_UNIVERSAL_TIME_OFFSET ( 0, 0, .AHEAD. ) ;
#1684 = VERTEX_POINT ( 'NONE', #3963 ) ;
#1685 = ADVANCED_FACE ( 'NONE', ( #1553 ), #7700, .F. ) ;
#1686 = DIRECTION ( 'NONE',  ( 0.000000000000000000, -1.000000000000000000, 0.000000000000000000 ) ) ;
#1687 = DIRECTION ( 'NONE',  ( -0.000000000000000000, -0.000000000000000000, 1.000000000000000000 ) ) ;
#1688 = DIRECTION ( 'NONE',  ( -0.000000000000000000, -1.000000000000000000, -0.000000000000000000 ) ) ;
#1689 = CC_DESIGN_PERSON_AND_ORGANIZATION_ASSIGNMENT ( #7879, #1051, ( #2972 ) ) ;
#1690 = EDGE_CURVE ( 'NONE', #4981, #358, #7076, .T. ) ;
#1691 = ADVANCED_FACE ( 'NONE', ( #5936, #3357 ), #802, .T. ) ;
#1692 = ORIENTED_EDGE ( 'NONE', *, *, #1424, .T. ) ;
#1693 = ORIENTED_EDGE ( 'NONE', *, *, #6397, .T. ) ;
#1694 = LINE ( 'NONE', #4198, #2268 ) ;
#1695 = CARTESIAN_POINT ( 'NONE',  ( -0.03921911030312481838, -0.4592703903598064352, 0.2500000000000000000 ) ) ;
#1696 = APPROVAL_STATUS ( 'not_yet_approved' ) ;
#1697 = CARTESIAN_POINT ( 'NONE',  ( 1.258671604940864608, -0.02501003737716508274, 5.393636709996481038 ) ) ;
#1698 = ORIENTED_EDGE ( 'NONE', *, *, #7985, .T. ) ;
#1699 = DIRECTION ( 'NONE',  ( 0.000000000000000000, 0.000000000000000000, 1.000000000000000000 ) ) ;
#1700 = DIRECTION ( 'NONE',  ( -1.000000000000000000, 0.000000000000000000, 0.000000000000000000 ) ) ;
#1701 = DIRECTION ( 'NONE',  ( 0.000000000000000000, 1.000000000000000000, 0.000000000000000000 ) ) ;
#1702 = PERSON_AND_ORGANIZATION ( #4735, #6190 ) ;
#1703 = FACE_OUTER_BOUND ( 'NONE', #2519, .T. ) ;
#1704 = CARTESIAN_POINT ( 'NONE',  ( 1.478057046718104228, 1.237683112344551084, 0.2500000000000000555 ) ) ;
#1705 = ORIENTED_EDGE ( 'NONE', *, *, #426, .T. ) ;
#1706 = CARTESIAN_POINT ( 'NONE',  ( 1.537507892858355873, 1.215016084663213869, 0.1879675853768330851 ) ) ;
#1707 = DIRECTION ( 'NONE',  ( -0.6568496200222107007, -0.7540216022612863389, 0.000000000000000000 ) ) ;
#1708 = PERSON ( 'NAUO-PER8', 'UNSPECIFIED', 'UNSPECIFIED', ('UNSPECIFIED'), ('UNSPECIFIED'), ('UNSPECIFIED') ) ;
#1709 = FACE_OUTER_BOUND ( 'NONE', #3841, .T. ) ;
#1710 = CARTESIAN_POINT ( 'NONE',  ( 0.1028096983035132889, -0.4582465879184300372, 0.2500000000000000000 ) ) ;
#1711 = CARTESIAN_POINT ( 'NONE',  ( 0.000000000000000000, 0.6124999999999999334, 0.1250000000000000000 ) ) ;
#1712 = ORIENTED_EDGE ( 'NONE', *, *, #989, .T. ) ;
#1713 = ORIENTED_EDGE ( 'NONE', *, *, #5177, .F. ) ;
#1714 = PLANE ( 'NONE',  #3573 ) ;
#1715 = DIRECTION ( 'NONE',  ( 1.000000000000000000, 0.000000000000000000, 0.000000000000000000 ) ) ;
#1716 = DIRECTION ( 'NONE',  ( -1.000000000000000000, 0.000000000000000000, 0.000000000000000000 ) ) ;
#1717 = APPROVAL_ROLE ( '' ) ;
#1718 = ORIENTED_EDGE ( 'NONE', *, *, #3260, .T. ) ;
#1719 = DIRECTION ( 'NONE',  ( -0.000000000000000000, 0.000000000000000000, 1.000000000000000000 ) ) ;
#1720 =( BOUNDED_CURVE ( )  B_SPLINE_CURVE ( 3, ( #748, #2060, #5781, #1350 ),
 .UNSPECIFIED., .F., .T. ) 
 B_SPLINE_CURVE_WITH_KNOTS ( ( 4, 4 ),
 ( 3.141592653589793116, 4.712388980384674575 ),
 .UNSPECIFIED. ) 
 CURVE ( )  GEOMETRIC_REPRESENTATION_ITEM ( )  RATIONAL_B_SPLINE_CURVE ( ( 1.000000000000000000, 0.8047378541243684902, 0.8047378541243684902, 1.000000000000000000 ) ) 
 REPRESENTATION_ITEM ( '' )  );
#1721 = CARTESIAN_POINT ( 'NONE',  ( 0.9207653111462810180, 0.7459592875503607834, 0.2500000000000000000 ) ) ;
#1722 = PLANE ( 'NONE',  #1994 ) ;
#1723 = EDGE_CURVE ( 'NONE', #358, #4885, #5242, .T. ) ;
#1724 = EDGE_CURVE ( 'NONE', #6311, #6574, #7728, .T. ) ;
#1725 = ADVANCED_FACE ( 'NONE', ( #7122 ), #3431, .T. ) ;
#1726 =( GEOMETRIC_REPRESENTATION_CONTEXT ( 3 ) GLOBAL_UNCERTAINTY_ASSIGNED_CONTEXT ( ( #6220 ) ) GLOBAL_UNIT_ASSIGNED_CONTEXT ( ( #2225, #5922, #964 ) ) REPRESENTATION_CONTEXT ( 'NONE', 'WORKASPACE' ) );
#1727 = CC_DESIGN_APPROVAL ( #89, ( #418 ) ) ;
#1728 = ORIENTED_EDGE ( 'NONE', *, *, #4183, .T. ) ;
#1729 = AXIS2_PLACEMENT_3D ( 'NONE', #6310, #767, #1336 ) ;
#1730 = CC_DESIGN_PERSON_AND_ORGANIZATION_ASSIGNMENT ( #2629, #1404, ( #4611 ) ) ;
#1731 = EDGE_CURVE ( 'NONE', #845, #6740, #4546, .T. ) ;
#1732 = ORIENTED_EDGE ( 'NONE', *, *, #5123, .F. ) ;
#1733 = CARTESIAN_POINT ( 'NONE',  ( 1.684866161243239846, 1.178252195112418299, -0.1039999999999998703 ) ) ;
#1734 = CARTESIAN_POINT ( 'NONE',  ( 0.07619294758106566479, -0.4615701726917245673, 0.2315531569361643227 ) ) ;
#1735 = CALENDAR_DATE ( 2026, 9, 10 ) ;
#1736 = DIRECTION ( 'NONE',  ( -0.000000000000000000, -0.000000000000000000, 1.000000000000000000 ) ) ;
#1737 = AXIS2_PLACEMENT_3D ( 'NONE', #4102, #5912, #6026 ) ;
#1738 = ORIENTED_EDGE ( 'NONE', *, *, #7090, .F. ) ;
#1739 = EDGE_LOOP ( 'NONE', ( #3323, #1670, #7024, #7032, #5755 ) ) ;
#1740 = CARTESIAN_POINT ( 'NONE',  ( 1.329175868372617808, 1.071828013948508573, -0.09195621454640677539 ) ) ;
#1741 = CYLINDRICAL_SURFACE ( 'NONE', #7289, 3.939999999999463487 ) ;
#1742 = AXIS2_PLACEMENT_3D ( 'NONE', #6564, #3976, #5257 ) ;
#1743 = CARTESIAN_POINT ( 'NONE',  ( 0.05830766503004893714, -0.4630768614767043490, 0.01347280640398593708 ) ) ;
#1744 = APPLICATION_PROTOCOL_DEFINITION ( 'international standard', 'config_control_design', 1994, #7659 ) ;
#1745 = CARTESIAN_POINT ( 'NONE',  ( 0.06250000000000000000, 7.654042494670957545E-18, 0.1250000000000000278 ) ) ;
#1746 = CARTESIAN_POINT ( 'NONE',  ( -1.723766588794375387, 1.115324847714046497, 0.1339999999999995361 ) ) ;
#1747 = ORIENTED_EDGE ( 'NONE', *, *, #1723, .T. ) ;
#1748 = CARTESIAN_POINT ( 'NONE',  ( 1.621822537759170402, 1.217706612625922613, 0.1978325958163386078 ) ) ;
#1749 = DIRECTION ( 'NONE',  ( 0.000000000000000000, 0.000000000000000000, 1.000000000000000000 ) ) ;
#1750 = ORIENTED_EDGE ( 'NONE', *, *, #1723, .F. ) ;
#1751 = DIRECTION ( 'NONE',  ( 0.000000000000000000, 0.000000000000000000, 1.000000000000000000 ) ) ;
#1752 = FACE_OUTER_BOUND ( 'NONE', #923, .T. ) ;
#1753 = CIRCLE ( 'NONE', #2665, 9.064497838702109789 ) ;
#1754 = VECTOR ( 'NONE', #903, 39.37007874015748143 ) ;
#1755 = CARTESIAN_POINT ( 'NONE',  ( -0.1250000000000000000, 0.5625000000000000000, 0.03125000000000000000 ) ) ;
#1756 = VERTEX_POINT ( 'NONE', #2167 ) ;
#1757 = EDGE_LOOP ( 'NONE', ( #1640, #5600, #2195, #3060 ) ) ;
#1758 = DIRECTION ( 'NONE',  ( 1.000000000000000000, 0.000000000000000000, 0.000000000000000000 ) ) ;
#1759 = CIRCLE ( 'NONE', #7264, 0.1150000000000000050 ) ;
#1760 = DIRECTION ( 'NONE',  ( -0.7879377495398142139, -0.6157549048526800295, 0.000000000000000000 ) ) ;
#1761 = DIRECTION ( 'NONE',  ( -0.000000000000000000, -1.000000000000000000, -0.000000000000000000 ) ) ;
#1762 = APPROVAL_DATE_TIME ( #4272, #7704 ) ;
#1763 = ORIENTED_EDGE ( 'NONE', *, *, #884, .T. ) ;
#1764 = DIRECTION ( 'NONE',  ( 0.000000000000000000, -1.000000000000000000, -0.000000000000000000 ) ) ;
#1765 = DIRECTION ( 'NONE',  ( 0.000000000000000000, -1.000000000000000000, -0.000000000000000000 ) ) ;
#1766 = VECTOR ( 'NONE', #6054, 39.37007874015748143 ) ;
#1767 = VECTOR ( 'NONE', #5620, 39.37007874015748143 ) ;
#1768 = ORIENTED_EDGE ( 'NONE', *, *, #6204, .F. ) ;
#1769 = DIRECTION ( 'NONE',  ( -0.000000000000000000, -0.000000000000000000, -1.000000000000000000 ) ) ;
#1770 = ORIENTED_EDGE ( 'NONE', *, *, #5789, .F. ) ;
#1771 = AXIS2_PLACEMENT_3D ( 'NONE', #5011, #4858, #4285 ) ;
#1772 = LINE ( 'NONE', #2417, #5060 ) ;
#1773 = EDGE_CURVE ( 'NONE', #2220, #6593, #940, .T. ) ;
#1774 = FACE_OUTER_BOUND ( 'NONE', #4349, .T. ) ;
#1775 = APPROVAL_ROLE ( '' ) ;
#1776 = DIRECTION ( 'NONE',  ( -0.000000000000000000, 1.000000000000000000, -0.000000000000000000 ) ) ;
#1777 = EDGE_CURVE ( 'NONE', #1231, #6526, #2639, .T. ) ;
#1778 = AXIS2_PLACEMENT_3D ( 'NONE', #1438, #4474, #3284 ) ;
#1779 = ORIENTED_EDGE ( 'NONE', *, *, #6697, .F. ) ;
#1780 = FACE_OUTER_BOUND ( 'NONE', #8091, .T. ) ;
#1781 = VECTOR ( 'NONE', #7133, 39.37007874015748143 ) ;
#1782 = LINE ( 'NONE', #4251, #6641 ) ;
#1783 = ADVANCED_FACE ( 'NONE', ( #2207 ), #7203, .T. ) ;
#1784 = EDGE_CURVE ( 'NONE', #6037, #3726, #7871, .T. ) ;
#1785 = CARTESIAN_POINT ( 'NONE',  ( 0.7938352818579558212, 1.310043527237274574, -0.3750000000000000555 ) ) ;
#1786 = CALENDAR_DATE ( 2026, 9, 10 ) ;
#1787 = CARTESIAN_POINT ( 'NONE',  ( 6.317381622560545473, 0.2407432673787524013, -0.1849999999999999978 ) ) ;
#1788 = CARTESIAN_POINT ( 'NONE',  ( 1.475891671935536609, 0.7226544316391472211, 0.1849999999999999978 ) ) ;
#1789 = ORIENTED_EDGE ( 'NONE', *, *, #376, .F. ) ;
#1790 = AXIS2_PLACEMENT_3D ( 'NONE', #1710, #5447, #604 ) ;
#1791 = VECTOR ( 'NONE', #5009, 39.37007874015748143 ) ;
#1792 = CARTESIAN_POINT ( 'NONE',  ( -6.110602001756019419, -1.404684638105634820, 0.000000000000000000 ) ) ;
#1793 = DIRECTION ( 'NONE',  ( 0.7540216022612863389, -0.6568496200222107007, 0.000000000000000000 ) ) ;
#1794 = CC_DESIGN_PERSON_AND_ORGANIZATION_ASSIGNMENT ( #547, #219, ( #1211 ) ) ;
#1795 = ADVANCED_FACE ( 'NONE', ( #6667 ), #5664, .T. ) ;
#1796 = CIRCLE ( 'NONE', #6374, 8.573908398499121120 ) ;
#1797 = ORIENTED_EDGE ( 'NONE', *, *, #7351, .F. ) ;
#1798 = FACE_OUTER_BOUND ( 'NONE', #3350, .T. ) ;
#1799 = CARTESIAN_POINT ( 'NONE',  ( 1.293421091588340621, 1.088624948896591560, -0.1020512680642866737 ) ) ;
#1800 = CARTESIAN_POINT ( 'NONE',  ( 1.515601125127084003, 1.045975532051838908, -0.1039999999999998287 ) ) ;
#1801 = ORIENTED_EDGE ( 'NONE', *, *, #1275, .T. ) ;
#1802 = ORIENTED_EDGE ( 'NONE', *, *, #1531, .F. ) ;
#1803 = VECTOR ( 'NONE', #7599, 39.37007874015748143 ) ;
#1804 = DIRECTION ( 'NONE',  ( -0.000000000000000000, -0.000000000000000000, 1.000000000000000000 ) ) ;
#1805 = VECTOR ( 'NONE', #7718, 39.37007874015748143 ) ;
#1806 = FACE_OUTER_BOUND ( 'NONE', #5859, .T. ) ;
#1807 = CARTESIAN_POINT ( 'NONE',  ( 0.1255000000000000282, 1.916572240665608148E-17, -0.5599999999999999423 ) ) ;
#1808 = PERSON_AND_ORGANIZATION ( #4735, #6190 ) ;
#1809 = ORIENTED_EDGE ( 'NONE', *, *, #3992, .F. ) ;
#1810 = FACE_OUTER_BOUND ( 'NONE', #1179, .T. ) ;
#1811 = DIRECTION ( 'NONE',  ( 0.000000000000000000, -0.000000000000000000, 1.000000000000000000 ) ) ;
#1812 = ORIENTED_EDGE ( 'NONE', *, *, #8086, .F. ) ;
#1813 = DIRECTION ( 'NONE',  ( -0.000000000000000000, 0.000000000000000000, 1.000000000000000000 ) ) ;
#1814 = EDGE_LOOP ( 'NONE', ( #1467, #6817, #4111, #2431 ) ) ;
#1815 = CARTESIAN_POINT ( 'NONE',  ( -0.9280291358773672394, 0.8548654847802351631, 0.09374999999999998612 ) ) ;
#1816 = LINE ( 'NONE', #6691, #2658 ) ;
#1817 = DIRECTION ( 'NONE',  ( 0.000000000000000000, 1.000000000000000000, -0.000000000000000000 ) ) ;
#1818 = ORIENTED_EDGE ( 'NONE', *, *, #272, .T. ) ;
#1819 = ADVANCED_FACE ( 'NONE', ( #7241 ), #7883, .F. ) ;
#1820 = ORIENTED_EDGE ( 'NONE', *, *, #7744, .F. ) ;
#1821 = CARTESIAN_POINT ( 'NONE',  ( 1.334235202004373511, 1.071904105284835262, -0.09796254303978589595 ) ) ;
#1822 = DIRECTION ( 'NONE',  ( -0.000000000000000000, -0.000000000000000000, -1.000000000000000000 ) ) ;
#1823 = EDGE_LOOP ( 'NONE', ( #6295, #3276, #1407, #3297 ) ) ;
#1824 = CARTESIAN_POINT ( 'NONE',  ( 0.1028096983035134415, -0.4582465879184300372, 0.03199999999999999373 ) ) ;
#1825 = COORDINATED_UNIVERSAL_TIME_OFFSET ( 0, 0, .AHEAD. ) ;
#1826 = CARTESIAN_POINT ( 'NONE',  ( 3.672798492683009286, -8.252032378159654513, 0.1850000000000003586 ) ) ;
#1827 = FACE_OUTER_BOUND ( 'NONE', #3699, .T. ) ;
#1828 = CARTESIAN_POINT ( 'NONE',  ( -0.9142296270274463676, 0.5739542246721701657, -0.09374999999999998612 ) ) ;
#1829 = EDGE_CURVE ( 'NONE', #3995, #1575, #5480, .T. ) ;
#1830 = ADVANCED_FACE ( 'NONE', ( #2275, #4212 ), #2934, .F. ) ;
#1831 = ORIENTED_EDGE ( 'NONE', *, *, #6391, .F. ) ;
#1832 = CARTESIAN_POINT ( 'NONE',  ( 0.03125000000000000000, -0.03125000000000000000, -0.1162848326531996102 ) ) ;
#1833 = CC_DESIGN_DATE_AND_TIME_ASSIGNMENT ( #2464, #2501, ( #3335 ) ) ;
#1834 = DIRECTION ( 'NONE',  ( 0.000000000000000000, 0.000000000000000000, -1.000000000000000000 ) ) ;
#1835 = EDGE_CURVE ( 'NONE', #3658, #6616, #1020, .T. ) ;
#1836 = EDGE_CURVE ( 'NONE', #340, #1448, #8003, .T. ) ;
#1837 = CARTESIAN_POINT ( 'NONE',  ( 1.356840083662244956, 0.003162463486408387866, 0.1250000000000000278 ) ) ;
#1838 = ORIENTED_EDGE ( 'NONE', *, *, #1085, .T. ) ;
#1839 = ORIENTED_EDGE ( 'NONE', *, *, #5487, .F. ) ;
#1840 = FACE_BOUND ( 'NONE', #5319, .T. ) ;
#1841 = CARTESIAN_POINT ( 'NONE',  ( 0.6597999294535048520, -0.04777128394798136474, 0.07449999999999999678 ) ) ;
#1842 = DIRECTION ( 'NONE',  ( 0.000000000000000000, 0.000000000000000000, -1.000000000000000000 ) ) ;
#1843 = PERSON_AND_ORGANIZATION_ROLE ( 'creator' ) ;
#1844 = ORIENTED_EDGE ( 'NONE', *, *, #7786, .T. ) ;
#1845 = CARTESIAN_POINT ( 'NONE',  ( 0.000000000000000000, 0.000000000000000000, -0.6229999999999998872 ) ) ;
#1846 = CARTESIAN_POINT ( 'NONE',  ( 1.537935346170436812, 1.852967428140057216, 0.000000000000000000 ) ) ;
#1847 = ORIENTED_EDGE ( 'NONE', *, *, #5217, .T. ) ;
#1848 = DIRECTION ( 'NONE',  ( -0.2873478855663425535, 0.000000000000000000, -0.9578262852211522071 ) ) ;
#1849 = EDGE_LOOP ( 'NONE', ( #5180, #3452, #5025, #5421, #5082, #3393, #7960, #2688, #5587, #1763, #760, #2743 ) ) ;
#1850 = CARTESIAN_POINT ( 'NONE',  ( 3.672798492683009286, -8.252032378159654513, 0.1250000000000004441 ) ) ;
#1851 = FACE_OUTER_BOUND ( 'NONE', #1757, .T. ) ;
#1852 = SECURITY_CLASSIFICATION_LEVEL ( 'unclassified' ) ;
#1853 = LINE ( 'NONE', #632, #596 ) ;
#1854 = AXIS2_PLACEMENT_3D ( 'NONE', #3869, #5639, #7596 ) ;
#1855 = ORIENTED_EDGE ( 'NONE', *, *, #7975, .F. ) ;
#1856 = VERTEX_POINT ( 'NONE', #7285 ) ;
#1857 = PRODUCT_DEFINITION_FORMATION_WITH_SPECIFIED_SOURCE ( 'ANY', '', #6511, .NOT_KNOWN. ) ;
#1858 = DIRECTION ( 'NONE',  ( -0.000000000000000000, -0.000000000000000000, 1.000000000000000000 ) ) ;
#1859 = DIRECTION ( 'NONE',  ( -1.000000000000000000, 0.000000000000000000, 0.000000000000000000 ) ) ;
#1860 = UNCERTAINTY_MEASURE_WITH_UNIT (LENGTH_MEASURE( 1.000000000000000082E-05 ), #3627, 'distance_accuracy_value', 'NONE');
#1861 = CARTESIAN_POINT ( 'NONE',  ( 0.1014930221493801354, -0.4584436548183983828, 0.02922833221147581179 ) ) ;
#1862 = CALENDAR_DATE ( 2026, 9, 10 ) ;
#1863 = CARTESIAN_POINT ( 'NONE',  ( -1.543211452806561690, 0.6927940070358462599, -0.1250000000000000000 ) ) ;
#1864 = CARTESIAN_POINT ( 'NONE',  ( 1.781235495941194680, 1.573674324865669938, -8.161306669393017495E-14 ) ) ;
#1865 = VECTOR ( 'NONE', #4057, 39.37007874015748143 ) ;
#1866 = LINE ( 'NONE', #1355, #34 ) ;
#1867 = LOCAL_TIME ( 14, 45, 32.00000000000000000, #835 ) ;
#1868 = VECTOR ( 'NONE', #202, 39.37007874015748143 ) ;
#1869 = VERTEX_POINT ( 'NONE', #2241 ) ;
#1870 = DIRECTION ( 'NONE',  ( -0.9578262852211522071, 0.000000000000000000, -0.2873478855663426645 ) ) ;
#1871 = CARTESIAN_POINT ( 'NONE',  ( 1.345270796830296378, 1.086053773142332757, -0.1449383704060485945 ) ) ;
#1872 = ADVANCED_FACE ( 'NONE', ( #6105 ), #3621, .F. ) ;
#1873 = ADVANCED_FACE ( 'NONE', ( #599 ), #5753, .T. ) ;
#1874 = CARTESIAN_POINT ( 'NONE',  ( -1.479329383613507964, -3.808562985511015242, 0.000000000000000000 ) ) ;
#1875 = VERTEX_POINT ( 'NONE', #6868 ) ;
#1876 = ADVANCED_FACE ( 'NONE', ( #786, #5562 ), #1439, .F. ) ;
#1877 = AXIS2_PLACEMENT_3D ( 'NONE', #854, #5860, #237 ) ;
#1878 = CYLINDRICAL_SURFACE ( 'NONE', #1343, 8.573908398499121120 ) ;
#1879 = EDGE_CURVE ( 'NONE', #1614, #7167, #6189, .T. ) ;
#1880 = EDGE_CURVE ( 'NONE', #4588, #3919, #159, .T. ) ;
#1881 = VECTOR ( 'NONE', #3647, 39.37007874015748143 ) ;
#1882 = VECTOR ( 'NONE', #1664, 39.37007874015748143 ) ;
#1883 = ORIENTED_EDGE ( 'NONE', *, *, #6393, .T. ) ;
#1884 = DIRECTION ( 'NONE',  ( -1.000000000000000000, 6.975840231036812635E-15, 0.000000000000000000 ) ) ;
#1885 = DIRECTION ( 'NONE',  ( 0.000000000000000000, 0.000000000000000000, -1.000000000000000000 ) ) ;
#1886 = CALENDAR_DATE ( 2026, 9, 10 ) ;
#1887 = EDGE_CURVE ( 'NONE', #4149, #5293, #410, .T. ) ;
#1888 = EDGE_LOOP ( 'NONE', ( #6030, #379, #387, #7947, #6151, #7268, #5762, #6134 ) ) ;
#1889 = CARTESIAN_POINT ( 'NONE',  ( -0.06999999999999996503, 0.03125000000000000000, 0.8125000000000000000 ) ) ;
#1890 = CARTESIAN_POINT ( 'NONE',  ( -1.203304165734202735, -0.2076492422562720153, 0.2349865476952187893 ) ) ;
#1891 = ORIENTED_EDGE ( 'NONE', *, *, #2363, .T. ) ;
#1892 = CARTESIAN_POINT ( 'NONE',  ( 4.405984854984288823, -2.483262103238899954, 0.1250000000000000000 ) ) ;
#1893 = AXIS2_PLACEMENT_3D ( 'NONE', #5181, #7563, #55 ) ;
#1894 = LOCAL_TIME ( 14, 45, 32.00000000000000000, #5427 ) ;
#1895 = AXIS2_PLACEMENT_3D ( 'NONE', #6015, #6516, #1619 ) ;
#1896 = CC_DESIGN_PERSON_AND_ORGANIZATION_ASSIGNMENT ( #4561, #6536, ( #5404 ) ) ;
#1897 = ORIENTED_EDGE ( 'NONE', *, *, #374, .T. ) ;
#1898 = DIRECTION ( 'NONE',  ( 1.000000000000000000, 0.000000000000000000, 0.000000000000000000 ) ) ;
#1899 = CIRCLE ( 'NONE', #855, 0.1249999999999998473 ) ;
#1900 = DIRECTION ( 'NONE',  ( -0.6568496200222107007, -0.7540216022612863389, -1.582067810090848267E-15 ) ) ;
#1901 = DIRECTION ( 'NONE',  ( -0.000000000000000000, 1.000000000000000000, -0.000000000000000000 ) ) ;
#1902 = CIRCLE ( 'NONE', #2016, 0.3750000000000000555 ) ;
#1903 = CARTESIAN_POINT ( 'NONE',  ( 1.877707900143042563, 1.420965844381539167, -0.06059890939898970180 ) ) ;
#1904 = AXIS2_PLACEMENT_3D ( 'NONE', #350, #261, #5361 ) ;
#1905 = ORIENTED_EDGE ( 'NONE', *, *, #4342, .T. ) ;
#1906 = CARTESIAN_POINT ( 'NONE',  ( 5.983714301115758083, -0.05774751952986264397, 5.393636709996481038 ) ) ;
#1907 =( LENGTH_UNIT ( ) NAMED_UNIT ( * ) SI_UNIT ( $, .METRE. ) );
#1908 = CARTESIAN_POINT ( 'NONE',  ( -1.750746777110393282, 1.631196835986985505, 0.3125000000000000000 ) ) ;
#1909 = COORDINATED_UNIVERSAL_TIME_OFFSET ( 0, 0, .AHEAD. ) ;
#1910 = CARTESIAN_POINT ( 'NONE',  ( 0.9207653111462810180, 0.7459592875503607834, 0.2500000000000000000 ) ) ;
#1911 = CARTESIAN_POINT ( 'NONE',  ( 1.674724282714340262, 1.670501082519673330, -0.02948104019479953763 ) ) ;
#1912 = AXIS2_PLACEMENT_3D ( 'NONE', #2720, #5231, #5428 ) ;
#1913 = VERTEX_POINT ( 'NONE', #171 ) ;
#1914 = CIRCLE ( 'NONE', #867, 0.1250000000000000000 ) ;
#1915 = ORIENTED_EDGE ( 'NONE', *, *, #2015, .F. ) ;
#1917 = DIRECTION ( 'NONE',  ( -0.000000000000000000, 1.000000000000000000, -0.000000000000000000 ) ) ;
#1916 = AXIS2_PLACEMENT_3D ( 'NONE', #2695, #77, #772 ) ;
#1918 = CARTESIAN_POINT ( 'NONE',  ( 1.258616368121236118, -0.02482036781376564805, -0.1250000000000000000 ) ) ;
#1919 = CIRCLE ( 'NONE', #7925, 0.1250000000000000000 ) ;
#1920 = LINE ( 'NONE', #3152, #6581 ) ;
#1921 = VERTEX_POINT ( 'NONE', #2666 ) ;
#1922 = FACE_BOUND ( 'NONE', #3834, .T. ) ;
#1923 = CIRCLE ( 'NONE', #7288, 9.064497838702109789 ) ;
#1924 = EDGE_CURVE ( 'NONE', #2842, #7766, #1459, .T. ) ;
#1925 = ORIENTED_EDGE ( 'NONE', *, *, #6442, .T. ) ;
#1926 = CARTESIAN_POINT ( 'NONE',  ( 3.666415866878781848, -8.185094079965441694, -0.1849999999999999978 ) ) ;
#1927 = CARTESIAN_POINT ( 'NONE',  ( -0.03125000000000000000, 0.7500000000000001110, 0.1106726592253027691 ) ) ;
#1928 = PERSON_AND_ORGANIZATION_ROLE ( 'design_owner' ) ;
#1929 = VERTEX_POINT ( 'NONE', #5224 ) ;
#1930 = DIRECTION ( 'NONE',  ( -0.7540216022612861169, 0.6568496200222108117, 0.000000000000000000 ) ) ;
#1931 = AXIS2_PLACEMENT_3D ( 'NONE', #7066, #5183, #5416 ) ;
#1932 = VECTOR ( 'NONE', #7304, 39.37007874015748143 ) ;
#1933 = ORIENTED_EDGE ( 'NONE', *, *, #4747, .T. ) ;
#1934 = CARTESIAN_POINT ( 'NONE',  ( 0.000000000000000000, 1.393749999999999822, -0.1799999999999999933 ) ) ;
#1935 = EDGE_CURVE ( 'NONE', #305, #4615, #1866, .T. ) ;
#1936 = EDGE_CURVE ( 'NONE', #2354, #3933, #4214, .T. ) ;
#1937 = DIRECTION ( 'NONE',  ( -0.4964005096718412946, -0.8680936205257682170, 0.000000000000000000 ) ) ;
#1938 = CARTESIAN_POINT ( 'NONE',  ( -4.352122087710502463, -0.2377406176185953846, 0.4047670380269003942 ) ) ;
#1939 = DIRECTION ( 'NONE',  ( 0.000000000000000000, -0.000000000000000000, 1.000000000000000000 ) ) ;
#1940 = DIRECTION ( 'NONE',  ( -0.4964005096718455134, -0.8680936205257656635, 0.000000000000000000 ) ) ;
#1941 = EDGE_CURVE ( 'NONE', #880, #3919, #2514, .T. ) ;
#1942 = SHAPE_REPRESENTATION ( 'Cleco, Handle, Rivet', ( #3555 ), #6058 ) ;
#1943 = VERTEX_POINT ( 'NONE', #2711 ) ;
#1944 = DIRECTION ( 'NONE',  ( 0.7879377495398141029, 0.6157549048526800295, 0.000000000000000000 ) ) ;
#1945 = COORDINATED_UNIVERSAL_TIME_OFFSET ( 0, 0, .AHEAD. ) ;
#1946 = CARTESIAN_POINT ( 'NONE',  ( 3.666415866878782737, -8.185094079965432812, 0.1849999999999999978 ) ) ;
#1947 = CARTESIAN_POINT ( 'NONE',  ( -0.5950975756886817125, 0.1840126700235228119, 0.2500000000000000000 ) ) ;
#1948 = EDGE_LOOP ( 'NONE', ( #3768, #3454, #4859, #7832 ) ) ;
#1949 = ORIENTED_EDGE ( 'NONE', *, *, #4798, .F. ) ;
#1950 = APPLICATION_CONTEXT ( 'configuration controlled 3d designs of mechanical parts and assemblies' ) ;
#1951 = CARTESIAN_POINT ( 'NONE',  ( 3.666415866878781848, -8.185094079965441694, -0.1849999999999999978 ) ) ;
#1952 = EDGE_LOOP ( 'NONE', ( #4874, #4730, #1224, #2728 ) ) ;
#1953 = CARTESIAN_POINT ( 'NONE',  ( 0.000000000000000000, 1.393749999999999822, 0.000000000000000000 ) ) ;
#1954 = CARTESIAN_POINT ( 'NONE',  ( 0.000000000000000000, 1.081250000000000044, 0.2112499999999999933 ) ) ;
#1955 = CARTESIAN_POINT ( 'NONE',  ( -1.803041671366328202, 1.104810305277057259, -0.3269762307749163877 ) ) ;
#1956 = ORIENTED_EDGE ( 'NONE', *, *, #6337, .F. ) ;
#1957 = DIRECTION ( 'NONE',  ( -1.000000000000000000, 0.000000000000000000, 0.000000000000000000 ) ) ;
#1958 = CARTESIAN_POINT ( 'NONE',  ( 0.000000000000000000, 0.03124999999999997571, 0.000000000000000000 ) ) ;
#1959 = CARTESIAN_POINT ( 'NONE',  ( 0.000000000000000000, 0.000000000000000000, 0.1250000000000000000 ) ) ;
#1960 = DATE_AND_TIME ( #3733, #287 ) ;
#1961 = ORIENTED_EDGE ( 'NONE', *, *, #4243, .F. ) ;
#1962 = CARTESIAN_POINT ( 'NONE',  ( 1.258132545478801489, 1.077561972973184234, -0.07313160851655174655 ) ) ;
#1963 = CARTESIAN_POINT ( 'NONE',  ( 0.000000000000000000, 0.7500000000000001110, 0.000000000000000000 ) ) ;
#1964 = LINE ( 'NONE', #5665, #1868 ) ;
#1965 = SPHERICAL_SURFACE ( 'NONE', #5454, 0.01652128394798136474 ) ;
#1966 = DIRECTION ( 'NONE',  ( 8.881784197001252323E-16, 1.387778780781445676E-15, -0.9999999999999998890 ) ) ;
#1967 = CARTESIAN_POINT ( 'NONE',  ( 2.023273750469992349E-18, -0.03125000000000000000, 0.6481068805941697653 ) ) ;
#1968 = ORIENTED_EDGE ( 'NONE', *, *, #6931, .T. ) ;
#1969 = CC_DESIGN_PERSON_AND_ORGANIZATION_ASSIGNMENT ( #2139, #7140, ( #4083 ) ) ;
#1970 = ORIENTED_EDGE ( 'NONE', *, *, #7974, .T. ) ;
#1971 = ADVANCED_FACE ( 'NONE', ( #2442 ), #7716, .T. ) ;
#1972 = CARTESIAN_POINT ( 'NONE',  ( -0.1250000000000000000, 0.6250000000000000000, -0.03125000000000000000 ) ) ;
#1973 = DIRECTION ( 'NONE',  ( 0.7879377495398137699, 0.6157549048526805846, 0.000000000000000000 ) ) ;
#1974 = CC_DESIGN_SECURITY_CLASSIFICATION ( #6959, ( #4083 ) ) ;
#1975 = SHAPE_DEFINITION_REPRESENTATION ( #5984, #2 ) ;
#1976 = DIRECTION ( 'NONE',  ( 0.8875604078987042733, -0.4606913525677314158, 0.000000000000000000 ) ) ;
#1977 = CARTESIAN_POINT ( 'NONE',  ( 3.659299226295303686, -8.245510427152350275, -0.1849999999999999978 ) ) ;
#1978 = EDGE_CURVE ( 'NONE', #813, #5374, #3966, .T. ) ;
#1979 =( BOUNDED_SURFACE ( )  B_SPLINE_SURFACE ( 3, 2, ( 
 ( #1421, #3312, #2777 ),
 ( #4504, #3927, #4581 ),
 ( #5814, #912, #5249 ),
 ( #1510, #5288, #194 ),
 ( #2694, #5207, #7703 ),
 ( #2085, #7080, #3363 ),
 ( #7778, #3968, #5863 ),
 ( #241, #2738, #7732 ),
 ( #1556, #2123, #3405 ),
 ( #2172, #396, #5332 ) ),
 .UNSPECIFIED., .F., .F., .F. ) 
 B_SPLINE_SURFACE_WITH_KNOTS ( ( 4, 2, 2, 2, 4 ),
 ( 3, 3 ),
 ( 3.474043806539870438, 3.783630100001075025, 4.093216393462279612, 4.402802686923484643, 4.712388980384689674 ),
 ( 0.000000000000000000, 1.000000000000000000 ),
 .UNSPECIFIED. ) 
 GEOMETRIC_REPRESENTATION_ITEM ( )  RATIONAL_B_SPLINE_SURFACE ( (
 ( 1.000000000000000000, 0.7246887769596790374, 1.000000000000000000),
 ( 1.000000000000000000, 0.7240706762976710786, 1.000000000000000000),
 ( 1.000000000000000000, 0.7231708462380681546, 1.000000000000000000),
 ( 1.000000000000000000, 0.7208914930597065673, 1.000000000000000000),
 ( 1.000000000000000000, 0.7195114720895853244, 1.000000000000000000),
 ( 1.000000000000000000, 0.7163941252002704596, 1.000000000000000000),
 ( 1.000000000000000000, 0.7146571679537656596, 1.000000000000000000),
 ( 1.000000000000000000, 0.7109849263087011373, 1.000000000000000000),
 ( 1.000000000000000000, 0.7090503513044520423, 1.000000000000000000),
 ( 1.000000000000000000, 0.7071067811865479058, 1.000000000000000000) ) ) 
 REPRESENTATION_ITEM ( '' )  SURFACE ( )  );
#1980 = AXIS2_PLACEMENT_3D ( 'NONE', #6410, #5179, #6297 ) ;
#1981 = ADVANCED_BREP_SHAPE_REPRESENTATION ( '', ( #3593, #3555 ), #553 ) ;
#1982 = LOCAL_TIME ( 14, 45, 32.00000000000000000, #7131 ) ;
#1983 = ORIENTED_EDGE ( 'NONE', *, *, #3983, .F. ) ;
#1984 = VERTEX_POINT ( 'NONE', #4812 ) ;
#1985 = DIRECTION ( 'NONE',  ( 0.6157549048526803626, -0.7879377495398141029, 0.000000000000000000 ) ) ;
#1986 = EDGE_LOOP ( 'NONE', ( #7378, #7954, #1484, #7990 ) ) ;
#1987 = CIRCLE ( 'NONE', #1729, 0.4999999999999997224 ) ;
#1988 = LINE ( 'NONE', #2034, #5551 ) ;
#1989 = CARTESIAN_POINT ( 'NONE',  ( 6.190221022838899856, 0.4584861219976859026, -0.1849999999999999978 ) ) ;
#1990 = APPROVAL_PERSON_ORGANIZATION ( #3939, #5128, #5221 ) ;
#1991 = LOCAL_TIME ( 14, 45, 32.00000000000000000, #2556 ) ;
#1992 = FACE_OUTER_BOUND ( 'NONE', #6458, .T. ) ;
#1993 = FACE_OUTER_BOUND ( 'NONE', #263, .T. ) ;
#1994 = AXIS2_PLACEMENT_3D ( 'NONE', #2342, #6125, #7340 ) ;
#1995 = CARTESIAN_POINT ( 'NONE',  ( 1.848680164946085336, 1.461834501516724449, 0.02980581276967405810 ) ) ;
#1996 = CARTESIAN_POINT ( 'NONE',  ( 0.1250000000000000000, 0.5625000000000000000, 0.03125000000000000000 ) ) ;
#1997 = PERSON_AND_ORGANIZATION ( #4735, #6190 ) ;
#1998 = ORIENTED_EDGE ( 'NONE', *, *, #4733, .T. ) ;
#1999 = CIRCLE ( 'NONE', #5141, 0.03125000000000000694 ) ;
#2000 = DIRECTION ( 'NONE',  ( -1.000000000000000000, 0.000000000000000000, 0.000000000000000000 ) ) ;
#2001 = CARTESIAN_POINT ( 'NONE',  ( 1.800320205903117809, 1.030513867073702627, -0.1039999999999998703 ) ) ;
#2002 = ORIENTED_EDGE ( 'NONE', *, *, #328, .F. ) ;
#2003 = CARTESIAN_POINT ( 'NONE',  ( 0.000000000000000000, 0.000000000000000000, 0.09374999999999998612 ) ) ;
#2004 = AXIS2_PLACEMENT_3D ( 'NONE', #966, #6617, #1007 ) ;
#2005 = CARTESIAN_POINT ( 'NONE',  ( 0.000000000000000000, 1.050000000000000044, 0.000000000000000000 ) ) ;
#2006 =( LENGTH_UNIT ( ) NAMED_UNIT ( * ) SI_UNIT ( $, .METRE. ) );
#2007 = DIRECTION ( 'NONE',  ( -1.000000000000000000, 0.000000000000000000, 0.000000000000000000 ) ) ;
#2008 = PERSON_AND_ORGANIZATION ( #1708, #7127 ) ;
#2009 = DIRECTION ( 'NONE',  ( -0.000000000000000000, -0.000000000000000000, -1.000000000000000000 ) ) ;
#2010 = CIRCLE ( 'NONE', #2276, 0.1250000000000000000 ) ;
#2011 = AXIS2_PLACEMENT_3D ( 'NONE', #3225, #1985, #4494 ) ;
#2012 = CARTESIAN_POINT ( 'NONE',  ( 1.682670780591506876, 1.262878425707093744, 0.1946946326293004792 ) ) ;
#2013 = CC_DESIGN_APPROVAL ( #4489, ( #187 ) ) ;
#2014 = ORIENTED_EDGE ( 'NONE', *, *, #4346, .T. ) ;
#2015 = EDGE_CURVE ( 'NONE', #5187, #6313, #5276, .T. ) ;
#2016 = AXIS2_PLACEMENT_3D ( 'NONE', #638, #7356, #3673 ) ;
#2017 = ORIENTED_EDGE ( 'NONE', *, *, #4054, .T. ) ;
#2018 = LINE ( 'NONE', #1972, #5124 ) ;
#2019 = ORIENTED_EDGE ( 'NONE', *, *, #5907, .F. ) ;
#2020 = CARTESIAN_POINT ( 'NONE',  ( 0.6597999294535048520, -0.01652128394798136821, 0.000000000000000000 ) ) ;
#2021 = DATE_AND_TIME ( #7681, #3044 ) ;
#2022 = CARTESIAN_POINT ( 'NONE',  ( 0.1028096983035134415, -0.4582465879184300372, 0.2179999999999999993 ) ) ;
#2023 = CARTESIAN_POINT ( 'NONE',  ( 1.353816004522938599, 0.002313473902802895728, -0.1850000000000455724 ) ) ;
#2024 = ORIENTED_EDGE ( 'NONE', *, *, #3533, .T. ) ;
#2025 = AXIS2_PLACEMENT_3D ( 'NONE', #7889, #5985, #2244 ) ;
#2026 = EDGE_CURVE ( 'NONE', #2766, #2552, #6571, .T. ) ;
#2027 = ADVANCED_FACE ( 'NONE', ( #925 ), #2914, .T. ) ;
#2028 = EDGE_CURVE ( 'NONE', #5362, #2657, #7145, .T. ) ;
#2029 = VERTEX_POINT ( 'NONE', #2912 ) ;
#2030 = CYLINDRICAL_SURFACE ( 'NONE', #2277, 9.004497838701052359 ) ;
#2031 = VECTOR ( 'NONE', #5390, 39.37007874015748143 ) ;
#2032 = ORIENTED_EDGE ( 'NONE', *, *, #7149, .F. ) ;
#2033 = ADVANCED_FACE ( 'NONE', ( #4718 ), #7544, .T. ) ;
#2034 = CARTESIAN_POINT ( 'NONE',  ( 1.347111479062088626E-17, 0.000000000000000000, -0.1100000000000000006 ) ) ;
#2035 = DIRECTION ( 'NONE',  ( -0.000000000000000000, 1.000000000000000000, -0.000000000000000000 ) ) ;
#2036 = APPROVAL ( #1292, 'UNSPECIFIED' ) ;
#2037 = DIRECTION ( 'NONE',  ( 0.7540216022612864499, -0.6568496200222104786, 0.000000000000000000 ) ) ;
#2038 = EDGE_CURVE ( 'NONE', #7840, #2261, #4191, .T. ) ;
#2039 = DIRECTION ( 'NONE',  ( -1.000000000000000000, 0.000000000000000000, 0.000000000000000000 ) ) ;
#2040 = CIRCLE ( 'NONE', #6360, 0.3024878104020024550 ) ;
#2041 = AXIS2_PLACEMENT_3D ( 'NONE', #7611, #4434, #5772 ) ;
#2042 = ORIENTED_EDGE ( 'NONE', *, *, #5043, .F. ) ;
#2043 = PRODUCT_DEFINITION_SHAPE ( 'NONE', 'NONE',  #8094 ) ;
#2044 = CARTESIAN_POINT ( 'NONE',  ( 1.860105863992942199, 1.471940519787515500, -0.01146616443475796492 ) ) ;
#2045 = DIRECTION ( 'NONE',  ( 1.000000000000000000, 0.000000000000000000, 0.000000000000000000 ) ) ;
#2046 = AXIS2_PLACEMENT_3D ( 'NONE', #1466, #5214, #1558 ) ;
#2047 = COORDINATED_UNIVERSAL_TIME_OFFSET ( 0, 0, .AHEAD. ) ;
#2048 = CARTESIAN_POINT ( 'NONE',  ( -0.04782642554762442377, -0.07812500000000000000, 0.000000000000000000 ) ) ;
#2049 = DIRECTION ( 'NONE',  ( 0.000000000000000000, 0.000000000000000000, -1.000000000000000000 ) ) ;
#2050 = CARTESIAN_POINT ( 'NONE',  ( 0.1210307295689817542, 0.6124999999999999334, -0.03125000000000000000 ) ) ;
#2051 = ORIENTED_EDGE ( 'NONE', *, *, #231, .T. ) ;
#2052 = CIRCLE ( 'NONE', #1388, 0.1487499999999999933 ) ;
#2053 = DIRECTION ( 'NONE',  ( -0.000000000000000000, -0.000000000000000000, 1.000000000000000000 ) ) ;
#2054 = AXIS2_PLACEMENT_3D ( 'NONE', #5119, #250, #7585 ) ;
#2055 = CIRCLE ( 'NONE', #361, 0.03199999999999997985 ) ;
#2056 = CARTESIAN_POINT ( 'NONE',  ( 0.2896281645421511231, -0.04777128394798136474, 0.07449999999999999678 ) ) ;
#2057 = AXIS2_PLACEMENT_3D ( 'NONE', #7401, #8078, #7357 ) ;
#2058 = CARTESIAN_POINT ( 'NONE',  ( 0.000000000000000000, 0.03125000000000000000, 0.2896281645421511231 ) ) ;
#2059 = APPROVAL_DATE_TIME ( #5916, #3691 ) ;
#2060 = CARTESIAN_POINT ( 'NONE',  ( -1.411633252941551175, 0.8434166392007481639, -0.1120558261758405477 ) ) ;
#2061 = CYLINDRICAL_SURFACE ( 'NONE', #1778, 0.1875000000000000278 ) ;
#2062 = CARTESIAN_POINT ( 'NONE',  ( 1.753077028676194526, 1.307477063583168064, 0.1680974545641061857 ) ) ;
#2063 = AXIS2_PLACEMENT_3D ( 'NONE', #3898, #3241, #3200 ) ;
#2064 = CIRCLE ( 'NONE', #4425, 0.1204106507132265275 ) ;
#2065 = DIRECTION ( 'NONE',  ( -0.000000000000000000, -0.000000000000000000, -1.000000000000000000 ) ) ;
#2066 = DIRECTION ( 'NONE',  ( 0.7531131608245043019, -0.6578909993250587895, 0.000000000000000000 ) ) ;
#2067 = DATE_TIME_ROLE ( 'classification_date' ) ;
#2068 = LINE ( 'NONE', #7761, #2443 ) ;
#2069 = DIRECTION ( 'NONE',  ( 0.7879377495398139919, 0.6157549048526802515, 0.000000000000000000 ) ) ;
#2070 = VERTEX_POINT ( 'NONE', #3497 ) ;
#2071 = ORIENTED_EDGE ( 'NONE', *, *, #6423, .T. ) ;
#2072 = ORIENTED_EDGE ( 'NONE', *, *, #1184, .T. ) ;
#2073 = EDGE_LOOP ( 'NONE', ( #3074, #5073 ) ) ;
#2074 = DIRECTION ( 'NONE',  ( 0.000000000000000000, 0.000000000000000000, 1.000000000000000000 ) ) ;
#2075 = VERTEX_POINT ( 'NONE', #878 ) ;
#2076 = CARTESIAN_POINT ( 'NONE',  ( 1.706166322112642630, 1.356275593161428983, 0.2051386464529749154 ) ) ;
#2077 = CARTESIAN_POINT ( 'NONE',  ( 1.393862768891835469, 1.061876785772673193, -0.1723397769375844824 ) ) ;
#2078 = CARTESIAN_POINT ( 'NONE',  ( 3.221700243049672174, 0.8684880333666047392, 0.1850000000000003586 ) ) ;
#2079 = EDGE_CURVE ( 'NONE', #6908, #112, #5876, .T. ) ;
#2080 = EDGE_CURVE ( 'NONE', #3032, #6429, #296, .T. ) ;
#2081 = CARTESIAN_POINT ( 'NONE',  ( -9.251037553912103917, -0.6017136928027502218, -0.05999999999999999778 ) ) ;
#2082 = B_SPLINE_CURVE_WITH_KNOTS ( 'NONE', 3,
 ( #2838, #7860, #293, #7097, #1602, #4763 ),
 .UNSPECIFIED., .F., .F.,
 ( 4, 2, 4 ),
 ( 6.316259036090116417E-16, 0.0006701634491691482601, 0.001340326898337664864 ),
 .UNSPECIFIED. ) ;
#2083 = ADVANCED_FACE ( 'NONE', ( #2874 ), #554, .T. ) ;
#2084 = EDGE_CURVE ( 'NONE', #6859, #1218, #7265, .T. ) ;
#2085 = CARTESIAN_POINT ( 'NONE',  ( 1.374642519223019832, 1.763930785958341962, 0.1748676107922683409 ) ) ;
#2086 = ADVANCED_FACE ( 'NONE', ( #4849 ), #1069, .F. ) ;
#2087 = CARTESIAN_POINT ( 'NONE',  ( 0.1250000000000000278, -0.03125000000000000000, 0.06250000000000000000 ) ) ;
#2088 = APPROVAL_ROLE ( '' ) ;
#2089 = VERTEX_POINT ( 'NONE', #624 ) ;
#2090 = DIRECTION ( 'NONE',  ( 1.000000000000000000, 0.000000000000000000, 0.000000000000000000 ) ) ;
#2091 = CARTESIAN_POINT ( 'NONE',  ( 0.3373886113636296868, -0.3568617631054005757, 0.008742659207913911629 ) ) ;
#2092 = ORIENTED_EDGE ( 'NONE', *, *, #4442, .T. ) ;
#2093 = LINE ( 'NONE', #1469, #7763 ) ;
#2094 = DIRECTION ( 'NONE',  ( 0.7879377495398142139, 0.6157549048526801405, 0.000000000000000000 ) ) ;
#2095 = CARTESIAN_POINT ( 'NONE',  ( 0.000000000000000000, 0.000000000000000000, 0.000000000000000000 ) ) ;
#2096 = APPROVAL_DATE_TIME ( #7713, #5128 ) ;
#2097 = ORIENTED_EDGE ( 'NONE', *, *, #2479, .F. ) ;
#2098 = PLANE ( 'NONE',  #2176 ) ;
#2099 = CARTESIAN_POINT ( 'NONE',  ( 1.717580241504790273, 1.374761148290041257, 0.1672982580699149402 ) ) ;
#2100 = ORIENTED_EDGE ( 'NONE', *, *, #1328, .F. ) ;
#2101 = DIRECTION ( 'NONE',  ( 0.9999999999999997780, 1.240231032643553605E-16, 9.121065767255463271E-17 ) ) ;
#2102 = CARTESIAN_POINT ( 'NONE',  ( -1.693368449338919598E-15, 1.112500000000000044, 0.2425000000000000211 ) ) ;
#2103 = FACE_OUTER_BOUND ( 'NONE', #6381, .T. ) ;
#2104 = APPLICATION_PROTOCOL_DEFINITION ( 'international standard', 'config_control_design', 1994, #1115 ) ;
#2105 = CARTESIAN_POINT ( 'NONE',  ( 0.1255000000000000282, 0.000000000000000000, 0.06300000000000000044 ) ) ;
#2106 = DIRECTION ( 'NONE',  ( -1.000000000000000000, 0.000000000000000000, 0.000000000000000000 ) ) ;
#2107 = ORIENTED_EDGE ( 'NONE', *, *, #4346, .F. ) ;
#2108 = ORIENTED_EDGE ( 'NONE', *, *, #5694, .F. ) ;
#2109 = PRODUCT_DEFINITION_SHAPE ( 'NONE', 'NONE',  #6001 ) ;
#2110 = ORIENTED_EDGE ( 'NONE', *, *, #6048, .F. ) ;
#2111 = VERTEX_POINT ( 'NONE', #5 ) ;
#2112 = CARTESIAN_POINT ( 'NONE',  ( 6.000000000000001776, 0.000000000000000000, -0.1250000000000004441 ) ) ;
#2113 = ORIENTED_EDGE ( 'NONE', *, *, #1579, .T. ) ;
#2114 = CARTESIAN_POINT ( 'NONE',  ( 1.710641181630429219, 1.387640563648149250, 0.2051014882331889944 ) ) ;
#2115 = DIRECTION ( 'NONE',  ( 0.6568496200222108117, 0.7540216022612861169, 0.000000000000000000 ) ) ;
#2116 = DIRECTION ( 'NONE',  ( 0.000000000000000000, 0.000000000000000000, -1.000000000000000000 ) ) ;
#2117 = VECTOR ( 'NONE', #3799, 39.37007874015748854 ) ;
#2118 = CYLINDRICAL_SURFACE ( 'NONE', #5811, 8.633908398497670333 ) ;
#2119 = CIRCLE ( 'NONE', #1208, 0.03200000000000003536 ) ;
#2120 = B_SPLINE_CURVE_WITH_KNOTS ( 'NONE', 3,
 ( #7759, #417, #5388, #4724, #7194, #4116, #6618, #7224 ),
 .UNSPECIFIED., .F., .F.,
 ( 4, 2, 2, 4 ),
 ( 1.109483187648633347E-17, 0.0003176057502265475989, 0.0006352115004530840305, 0.001270423000906161989 ),
 .UNSPECIFIED. ) ;
#2121 = ADVANCED_FACE ( 'NONE', ( #4886, #2495, #7428 ), #1722, .F. ) ;
#2122 =( GEOMETRIC_REPRESENTATION_CONTEXT ( 3 ) GLOBAL_UNCERTAINTY_ASSIGNED_CONTEXT ( ( #8080 ) ) GLOBAL_UNIT_ASSIGNED_CONTEXT ( ( #7387, #4891, #7344 ) ) REPRESENTATION_CONTEXT ( 'NONE', 'WORKASPACE' ) );
#2123 = CARTESIAN_POINT ( 'NONE',  ( 1.270760784386404385, 1.682749642158441361, 0.2498245760079802757 ) ) ;
#2124 = DIRECTION ( 'NONE',  ( 1.000000000000000000, 0.000000000000000000, 0.000000000000000000 ) ) ;
#2125 = PERSON_AND_ORGANIZATION ( #4735, #6190 ) ;
#2126 = CARTESIAN_POINT ( 'NONE',  ( 0.000000000000000000, 0.000000000000000000, -0.6849999999999999423 ) ) ;
#2127 = DIRECTION ( 'NONE',  ( 0.000000000000000000, -1.000000000000000000, 0.000000000000000000 ) ) ;
#2128 = DIRECTION ( 'NONE',  ( -0.000000000000000000, 0.000000000000000000, -1.000000000000000000 ) ) ;
#2129 = ORIENTED_EDGE ( 'NONE', *, *, #236, .F. ) ;
#2130 = CIRCLE ( 'NONE', #5802, 0.4060000000000000830 ) ;
#2131 = LINE ( 'NONE', #1517, #5674 ) ;
#2132 = APPROVAL ( #4807, 'UNSPECIFIED' ) ;
#2133 = LOCAL_TIME ( 14, 45, 32.00000000000000000, #7824 ) ;
#2134 = EDGE_CURVE ( 'NONE', #4364, #6669, #6584, .T. ) ;
#2135 = EDGE_CURVE ( 'NONE', #2575, #4907, #3036, .T. ) ;
#2136 = AXIS2_PLACEMENT_3D ( 'NONE', #8014, #4800, #3727 ) ;
#2137 = FACE_OUTER_BOUND ( 'NONE', #2907, .T. ) ;
#2138 = CARTESIAN_POINT ( 'NONE',  ( 0.000000000000000000, 1.112500000000000044, 0.000000000000000000 ) ) ;
#2139 = PERSON_AND_ORGANIZATION ( #4735, #6190 ) ;
#2140 = ORIENTED_EDGE ( 'NONE', *, *, #2188, .F. ) ;
#2141 = CARTESIAN_POINT ( 'NONE',  ( -0.03125000000000000000, 0.03124999999999997571, 0.1106726592253027830 ) ) ;
#2142 = CARTESIAN_POINT ( 'NONE',  ( 1.290272380711668720, -0.01560121663631008383, -0.1250000000000000278 ) ) ;
#2143 = CC_DESIGN_DATE_AND_TIME_ASSIGNMENT ( #773, #6843, ( #830 ) ) ;
#2144 = EDGE_CURVE ( 'NONE', #4981, #1649, #6729, .T. ) ;
#2145 = TOROIDAL_SURFACE ( 'NONE', #7513, 6.962657474112426748, 0.03200000000000000067 ) ;
#2146 = CIRCLE ( 'NONE', #1099, 0.4070000000000002505 ) ;
#2147 = FACE_OUTER_BOUND ( 'NONE', #7987, .T. ) ;
#2148 = VECTOR ( 'NONE', #3877, 39.37007874015748143 ) ;
#2149 = B_SPLINE_CURVE_WITH_KNOTS ( 'NONE', 3,
 ( #5084, #778, #3783, #3277, #1347, #4401 ),
 .UNSPECIFIED., .F., .F.,
 ( 4, 2, 4 ),
 ( 2.945200827377960913E-17, 0.001884585737150711168, 0.003769171474301399351 ),
 .UNSPECIFIED. ) ;
#2150 = DIRECTION ( 'NONE',  ( -0.6157549048526801405, 0.7879377495398142139, 0.000000000000000000 ) ) ;
#2151 = CALENDAR_DATE ( 2026, 9, 10 ) ;
#2152 = DIRECTION ( 'NONE',  ( -0.000000000000000000, -0.000000000000000000, 1.000000000000000000 ) ) ;
#2153 = ORIENTED_EDGE ( 'NONE', *, *, #2533, .F. ) ;
#2154 = ORIENTED_EDGE ( 'NONE', *, *, #4545, .T. ) ;
#2155 = VERTEX_POINT ( 'NONE', #3738 ) ;
#2156 = LOCAL_TIME ( 14, 45, 32.00000000000000000, #4972 ) ;
#2157 = AXIS2_PLACEMENT_3D ( 'NONE', #7997, #1858, #470 ) ;
#2158 = ORIENTED_EDGE ( 'NONE', *, *, #7741, .F. ) ;
#2159 = ORIENTED_EDGE ( 'NONE', *, *, #5595, .T. ) ;
#2160 = FACE_OUTER_BOUND ( 'NONE', #6951, .T. ) ;
#2161 = ORIENTED_EDGE ( 'NONE', *, *, #5250, .T. ) ;
#2162 = CARTESIAN_POINT ( 'NONE',  ( -1.256933281983527929E-15, 1.425000000000000044, 0.1799999999999999933 ) ) ;
#2163 = CARTESIAN_POINT ( 'NONE',  ( 1.451358053557619598, 1.823882180053259860, 0.1350113725148300858 ) ) ;
#2164 = CIRCLE ( 'NONE', #6742, 0.1150000000000000050 ) ;
#2165 = CIRCLE ( 'NONE', #3209, 0.1150000000000000050 ) ;
#2166 = B_SPLINE_CURVE_WITH_KNOTS ( 'NONE', 3,
 ( #1195, #3704, #579, #6254, #3130, #3084, #5590, #5629, #3820, #6322, #5088, #1474 ),
 .UNSPECIFIED., .F., .F.,
 ( 4, 2, 2, 2, 2, 4 ),
 ( 2.684845590619915053E-17, 0.001673132518879472293, 0.003346265037758917697, 0.004182831297198636063, 0.005019397556638355296, 0.006692530075517771210 ),
 .UNSPECIFIED. ) ;
#2167 = CARTESIAN_POINT ( 'NONE',  ( 0.000000000000000000, 0.6124999999999999334, 0.1100000000000000006 ) ) ;
#2168 = DIRECTION ( 'NONE',  ( 0.000000000000000000, 0.000000000000000000, -1.000000000000000000 ) ) ;
#2169 = EDGE_LOOP ( 'NONE', ( #1600, #413, #2917, #769, #7266, #3171 ) ) ;
#2170 = VECTOR ( 'NONE', #4319, 39.37007874015748143 ) ;
#2171 = VECTOR ( 'NONE', #4664, 39.37007874015748143 ) ;
#2172 = CARTESIAN_POINT ( 'NONE',  ( 1.240314151020239120, 1.658956310969642800, 0.2179999999999998883 ) ) ;
#2173 = FACE_OUTER_BOUND ( 'NONE', #7893, .T. ) ;
#2174 = CARTESIAN_POINT ( 'NONE',  ( -1.411841654243101596, 0.8435981834898315102, 0.1250000000000000000 ) ) ;
#2175 = CARTESIAN_POINT ( 'NONE',  ( 0.000000000000000000, 1.393749999999999822, 0.000000000000000000 ) ) ;
#2176 = AXIS2_PLACEMENT_3D ( 'NONE', #2258, #4597, #7185 ) ;
#2177 = ORIENTED_EDGE ( 'NONE', *, *, #2028, .T. ) ;
#2178 = CARTESIAN_POINT ( 'NONE',  ( 1.387804320626534915, 1.063587717045087144, -0.1645371419711735006 ) ) ;
#2179 = AXIS2_PLACEMENT_3D ( 'NONE', #2001, #4438, #703 ) ;
#2180 = CARTESIAN_POINT ( 'NONE',  ( 0.03125000000000000000, 0.03124999999999997571, 0.1106726592253027830 ) ) ;
#2181 = CARTESIAN_POINT ( 'NONE',  ( 1.516422131414766339, 1.874728233683303324, -0.007188475204957444839 ) ) ;
#2182 = PERSON_AND_ORGANIZATION ( #4735, #6190 ) ;
#2183 = ORIENTED_EDGE ( 'NONE', *, *, #1624, .F. ) ;
#2184 = AXIS2_PLACEMENT_3D ( 'NONE', #4795, #242, #6184 ) ;
#2185 = CIRCLE ( 'NONE', #7807, 0.03124999999999996184 ) ;
#2186 = CARTESIAN_POINT ( 'NONE',  ( 1.517943318015056109, 1.875917005398948456, 0.03199999999999999373 ) ) ;
#2187 = CARTESIAN_POINT ( 'NONE',  ( 1.517690421966769732, 1.264920623095007191, 0.2500000000000000000 ) ) ;
#2188 = EDGE_CURVE ( 'NONE', #7797, #695, #1257, .T. ) ;
#2189 = ADVANCED_FACE ( 'NONE', ( #5463 ), #2371, .T. ) ;
#2190 = EDGE_CURVE ( 'NONE', #6170, #4512, #5585, .T. ) ;
#2191 = VECTOR ( 'NONE', #7075, 39.37007874015748143 ) ;
#2192 = ORIENTED_EDGE ( 'NONE', *, *, #1289, .T. ) ;
#2193 = ADVANCED_FACE ( 'NONE', ( #6247 ), #3128, .T. ) ;
#2194 =( LENGTH_UNIT ( ) NAMED_UNIT ( * ) SI_UNIT ( $, .METRE. ) );
#2195 = ORIENTED_EDGE ( 'NONE', *, *, #6434, .T. ) ;
#2196 = DIRECTION ( 'NONE',  ( -0.9987955914953420278, -0.04906492035527816598, 0.000000000000000000 ) ) ;
#2197 = CONTEXT_DEPENDENT_SHAPE_REPRESENTATION ( #5143, #2043 ) ;
#2198 = LINE ( 'NONE', #7912, #7139 ) ;
#2199 = ORIENTED_EDGE ( 'NONE', *, *, #4483, .T. ) ;
#2200 = AXIS2_PLACEMENT_3D ( 'NONE', #2674, #2297, #2956 ) ;
#2201 = AXIS2_PLACEMENT_3D ( 'NONE', #348, #3539, #7315 ) ;
#2202 = ORIENTED_EDGE ( 'NONE', *, *, #4249, .T. ) ;
#2203 = EDGE_LOOP ( 'NONE', ( #3418, #180, #6480, #933 ) ) ;
#2204 = CARTESIAN_POINT ( 'NONE',  ( 0.000000000000000000, 0.03125000000000000000, 0.2896281645421511231 ) ) ;
#2205 = LINE ( 'NONE', #391, #2171 ) ;
#2206 = CARTESIAN_POINT ( 'NONE',  ( 0.1875000000000000278, 0.000000000000000000, -0.6219999999999999973 ) ) ;
#2207 = FACE_OUTER_BOUND ( 'NONE', #324, .T. ) ;
#2208 = EDGE_LOOP ( 'NONE', ( #7830, #4073, #8069, #1883 ) ) ;
#2209 = DIRECTION ( 'NONE',  ( -0.000000000000000000, -1.000000000000000000, -0.000000000000000000 ) ) ;
#2210 = ORIENTED_EDGE ( 'NONE', *, *, #2671, .F. ) ;
#2211 = EDGE_LOOP ( 'NONE', ( #2159, #2024, #6229, #3940, #6245, #5675 ) ) ;
#2212 = CARTESIAN_POINT ( 'NONE',  ( 1.475891671935536165, 0.7226544316391469991, 0.1120558261758407698 ) ) ;
#2213 = LINE ( 'NONE', #1058, #6891 ) ;
#2214 = DIRECTION ( 'NONE',  ( 0.000000000000000000, 0.000000000000000000, -1.000000000000000000 ) ) ;
#2215 = VERTEX_POINT ( 'NONE', #1194 ) ;
#2216 = CARTESIAN_POINT ( 'NONE',  ( 0.1250000000000000000, 0.6250000000000000000, 0.03125000000000000000 ) ) ;
#2217 = FACE_OUTER_BOUND ( 'NONE', #247, .T. ) ;
#2218 = PLANE ( 'NONE',  #627 ) ;
#2219 = SECURITY_CLASSIFICATION_LEVEL ( 'unclassified' ) ;
#2220 = VERTEX_POINT ( 'NONE', #3080 ) ;
#2221 = DIRECTION ( 'NONE',  ( 0.000000000000000000, -1.000000000000000000, 0.000000000000000000 ) ) ;
#2222 = CARTESIAN_POINT ( 'NONE',  ( 1.142655413120957197, 0.6307864494084283180, 0.2500000000000000000 ) ) ;
#2223 = ORIENTED_EDGE ( 'NONE', *, *, #4738, .T. ) ;
#2224 = ORIENTED_EDGE ( 'NONE', *, *, #1291, .F. ) ;
#2225 =( CONVERSION_BASED_UNIT ( 'INCH', #6575 ) LENGTH_UNIT ( ) NAMED_UNIT ( #6154 ) );
#2226 = ADVANCED_FACE ( 'NONE', ( #8023 ), #163, .T. ) ;
#2227 = ORIENTED_EDGE ( 'NONE', *, *, #3028, .F. ) ;
#2228 = CARTESIAN_POINT ( 'NONE',  ( 1.877707900143042563, 1.420965844381539167, -0.06059890939898970180 ) ) ;
#2229 = CARTESIAN_POINT ( 'NONE',  ( 0.02199364308835362672, -0.4639489453757028592, 0.2441666941616341957 ) ) ;
#2230 = CALENDAR_DATE ( 2026, 9, 10 ) ;
#2231 = DIRECTION ( 'NONE',  ( -0.000000000000000000, -0.000000000000000000, -1.000000000000000000 ) ) ;
#2232 = VERTEX_POINT ( 'NONE', #3570 ) ;
#2233 = ORIENTED_EDGE ( 'NONE', *, *, #7079, .F. ) ;
#2234 = CC_DESIGN_DATE_AND_TIME_ASSIGNMENT ( #4104, #6606, ( #6959 ) ) ;
#2235 = EDGE_CURVE ( 'NONE', #1607, #6273, #4616, .T. ) ;
#2236 = VERTEX_POINT ( 'NONE', #4929 ) ;
#2237 = DIRECTION ( 'NONE',  ( 0.7879377495398141029, 0.6157549048526802515, -0.000000000000000000 ) ) ;
#2238 = ADVANCED_FACE ( 'NONE', ( #572 ), #457, .F. ) ;
#2239 = DIRECTION ( 'NONE',  ( -0.9987955914953422498, -0.04906492035527344059, 0.000000000000000000 ) ) ;
#2240 = DIRECTION ( 'NONE',  ( 0.7540216022612862279, -0.6568496200222107007, 0.000000000000000000 ) ) ;
#2241 = CARTESIAN_POINT ( 'NONE',  ( 6.185915932928153005, 0.4597367884986204856, -0.1849999999999999978 ) ) ;
#2242 = LINE ( 'NONE', #6559, #5541 ) ;
#2243 = PRODUCT_DEFINITION_SHAPE ( 'NONE', 'NONE',  #8099 ) ;
#2244 = DIRECTION ( 'NONE',  ( -1.000000000000000000, 0.000000000000000000, -0.000000000000000000 ) ) ;
#2245 = LINE ( 'NONE', #6561, #4928 ) ;
#2246 = DIRECTION ( 'NONE',  ( -1.000000000000000000, 0.000000000000000000, 0.000000000000000000 ) ) ;
#2247 = EDGE_LOOP ( 'NONE', ( #6447, #7209, #228, #1718, #298, #1414, #6780, #7069, #6233 ) ) ;
#2248 = DIRECTION ( 'NONE',  ( 0.000000000000000000, 0.000000000000000000, -1.000000000000000000 ) ) ;
#2249 =( GEOMETRIC_REPRESENTATION_CONTEXT ( 3 ) GLOBAL_UNCERTAINTY_ASSIGNED_CONTEXT ( ( #3014 ) ) GLOBAL_UNIT_ASSIGNED_CONTEXT ( ( #1648, #5879, #4600 ) ) REPRESENTATION_CONTEXT ( 'NONE', 'WORKASPACE' ) );
#2250 = APPROVAL_PERSON_ORGANIZATION ( #5865, #6755, #6663 ) ;
#2251 = CC_DESIGN_APPROVAL ( #6687, ( #3702 ) ) ;
#2252 = CYLINDRICAL_SURFACE ( 'NONE', #5957, 0.03124999999999997571 ) ;
#2253 = CARTESIAN_POINT ( 'NONE',  ( 3.672798492683009286, -8.252032378159654513, 5.393636709996481038 ) ) ;
#2254 = CALENDAR_DATE ( 2026, 9, 10 ) ;
#2255 = ORIENTED_EDGE ( 'NONE', *, *, #2611, .F. ) ;
#2256 = AXIS2_PLACEMENT_3D ( 'NONE', #5858, #978, #5810 ) ;
#2257 = CARTESIAN_POINT ( 'NONE',  ( -1.803041671366328202, 1.104810305277057259, -0.3269762307749163877 ) ) ;
#2258 = CARTESIAN_POINT ( 'NONE',  ( 0.2935750530104211387, 0.05119392622207447063, 0.07449999999999999678 ) ) ;
#2259 = APPROVAL_PERSON_ORGANIZATION ( #747, #3436, #94 ) ;
#2260 = AXIS2_PLACEMENT_3D ( 'NONE', #3411, #4064, #3371 ) ;
#2261 = VERTEX_POINT ( 'NONE', #5778 ) ;
#2262 = VERTEX_POINT ( 'NONE', #743 ) ;
#2263 = DIRECTION ( 'NONE',  ( -1.000000000000000000, 0.000000000000000000, 0.000000000000000000 ) ) ;
#2264 = DIRECTION ( 'NONE',  ( -1.000000000000000000, 0.000000000000000000, 0.000000000000000000 ) ) ;
#2265 = FACE_OUTER_BOUND ( 'NONE', #7657, .T. ) ;
#2266 = CIRCLE ( 'NONE', #1219, 0.03200000000000005618 ) ;
#2267 = ORIENTED_EDGE ( 'NONE', *, *, #2429, .T. ) ;
#2268 = VECTOR ( 'NONE', #6039, 39.37007874015748143 ) ;
#2269 = CARTESIAN_POINT ( 'NONE',  ( 1.238969240134095040, 1.657905294597833201, 0.2179999999999999993 ) ) ;
#2270 = DIRECTION ( 'NONE',  ( 1.000000000000000000, 0.000000000000000000, 0.000000000000000000 ) ) ;
#2271 = PERSON_AND_ORGANIZATION_ROLE ( 'creator' ) ;
#2272 = CARTESIAN_POINT ( 'NONE',  ( 0.03125000000000000000, 0.000000000000000000, 0.000000000000000000 ) ) ;
#2273 = DIRECTION ( 'NONE',  ( -0.000000000000000000, -0.000000000000000000, -1.000000000000000000 ) ) ;
#2274 = ORIENTED_EDGE ( 'NONE', *, *, #6193, .F. ) ;
#2275 = FACE_BOUND ( 'NONE', #7466, .T. ) ;
#2276 = AXIS2_PLACEMENT_3D ( 'NONE', #109, #2640, #267 ) ;
#2277 = AXIS2_PLACEMENT_3D ( 'NONE', #1951, #6417, #3918 ) ;
#2278 = FACE_BOUND ( 'NONE', #4220, .T. ) ;
#2279 = LOCAL_TIME ( 14, 45, 32.00000000000000000, #2617 ) ;
#2280 = CIRCLE ( 'NONE', #5430, 0.1250000000000000000 ) ;
#2281 = ORIENTED_EDGE ( 'NONE', *, *, #6214, .T. ) ;
#2282 = DIRECTION ( 'NONE',  ( -0.7879377495398141029, -0.6157549048526801405, 0.000000000000000000 ) ) ;
#2283 = PRODUCT_RELATED_PRODUCT_CATEGORY ( 'detail', '', ( #2972 ) ) ;
#2284 = DIRECTION ( 'NONE',  ( -1.000000000000000000, 0.000000000000000000, 0.000000000000000000 ) ) ;
#2285 = ADVANCED_FACE ( 'NONE', ( #3244 ), #7014, .T. ) ;
#2286 = CARTESIAN_POINT ( 'NONE',  ( -0.03125000000000000000, -0.03125000000000000000, 0.1162848326531996240 ) ) ;
#2287 = EDGE_CURVE ( 'NONE', #1539, #5845, #3819, .T. ) ;
#2288 = ORIENTED_EDGE ( 'NONE', *, *, #5053, .T. ) ;
#2289 = CARTESIAN_POINT ( 'NONE',  ( 0.000000000000000000, 0.5625000000000000000, 0.000000000000000000 ) ) ;
#2290 = CLOSED_SHELL ( 'NONE', ( #5596, #3139, #6249, #4803, #4357, #2285, #5797, #3926, #4482, #2785, #4790, #2086, #622, #4490, #7641, #5384 ) ) ;
#2291 = AXIS2_PLACEMENT_3D ( 'NONE', #4433, #6238, #1884 ) ;
#2292 = CARTESIAN_POINT ( 'NONE',  ( 0.1000000000000000472, 0.03125000000000000000, 0.06250000000000000000 ) ) ;
#2293 = CARTESIAN_POINT ( 'NONE',  ( 0.1028096983035134415, -0.4582465879184300372, 0.2179999999999999993 ) ) ;
#2294 = AXIS2_PLACEMENT_3D ( 'NONE', #5099, #6950, #3343 ) ;
#2295 = COORDINATED_UNIVERSAL_TIME_OFFSET ( 0, 0, .AHEAD. ) ;
#2296 = ORIENTED_EDGE ( 'NONE', *, *, #170, .T. ) ;
#2297 = DIRECTION ( 'NONE',  ( -0.000000000000000000, 1.000000000000000000, -0.000000000000000000 ) ) ;
#2298 = SHAPE_REPRESENTATION ( 'Cleco, Fastener, Shell', ( #3555 ), #1726 ) ;
#2299 = DIRECTION ( 'NONE',  ( 1.000000000000000000, 0.000000000000000000, 0.000000000000000000 ) ) ;
#2300 = DIRECTION ( 'NONE',  ( 1.000000000000000000, 0.000000000000000000, 0.000000000000000000 ) ) ;
#2301 = AXIS2_PLACEMENT_3D ( 'NONE', #4518, #3330, #7060 ) ;
#2302 = ORIENTED_EDGE ( 'NONE', *, *, #3534, .F. ) ;
#2303 = AXIS2_PLACEMENT_3D ( 'NONE', #7291, #281, #5905 ) ;
#2304 = CIRCLE ( 'NONE', #6893, 8.573908398499121120 ) ;
#2305 = ORIENTED_EDGE ( 'NONE', *, *, #719, .T. ) ;
#2306 = CARTESIAN_POINT ( 'NONE',  ( -1.411633252941551619, 0.8434166392007494961, -0.09374999999999998612 ) ) ;
#2307 = CARTESIAN_POINT ( 'NONE',  ( -0.04782642554762441683, -0.03125000000000000000, 0.07449999999999999678 ) ) ;
#2308 = CALENDAR_DATE ( 2026, 9, 10 ) ;
#2309 = CARTESIAN_POINT ( 'NONE',  ( -0.3566525292043903339, -0.3408511508279103985, 0.1250000000000000000 ) ) ;
#2310 = AXIS2_PLACEMENT_3D ( 'NONE', #2859, #7812, #7170 ) ;
#2311 = EDGE_LOOP ( 'NONE', ( #222, #5656, #5206, #6873 ) ) ;
#2312 = EDGE_LOOP ( 'NONE', ( #4574, #6941, #4448, #7073 ) ) ;
#2313 = CARTESIAN_POINT ( 'NONE',  ( -3.165020334763531729, -1.163753072338894023, -0.1250000000000000000 ) ) ;
#2314 = CYLINDRICAL_SURFACE ( 'NONE', #3372, 0.09507037842118626347 ) ;
#2316 = CARTESIAN_POINT ( 'NONE',  ( 3.672767723898985537, -8.314396374632453401, 0.1250000000000000000 ) ) ;
#2315 = AXIS2_PLACEMENT_3D ( 'NONE', #4228, #7720, #3950 ) ;
#2317 = APPROVAL_DATE_TIME ( #2930, #2739 ) ;
#2318 = DIRECTION ( 'NONE',  ( 0.000000000000000000, -0.000000000000000000, 1.000000000000000000 ) ) ;
#2319 = CIRCLE ( 'NONE', #4555, 0.2112499999999999933 ) ;
#2320 = CARTESIAN_POINT ( 'NONE',  ( 1.457966743008886068, 1.224466284236799041, 0.2500000000000000000 ) ) ;
#2321 = EDGE_CURVE ( 'NONE', #789, #6740, #1338, .T. ) ;
#2322 = ADVANCED_FACE ( 'NONE', ( #160 ), #7547, .F. ) ;
#2323 = ORIENTED_EDGE ( 'NONE', *, *, #373, .T. ) ;
#2324 = CARTESIAN_POINT ( 'NONE',  ( 1.496290583815347741, 1.216672708051755647, 0.2341988374537135043 ) ) ;
#2325 = DIRECTION ( 'NONE',  ( 0.6157549048526801405, -0.7879377495398141029, 0.000000000000000000 ) ) ;
#2326 = CIRCLE ( 'NONE', #6911, 0.2112499999999999933 ) ;
#2327 = VERTEX_POINT ( 'NONE', #1934 ) ;
#2328 = DIRECTION ( 'NONE',  ( 1.000000000000000000, 0.000000000000000000, 0.000000000000000000 ) ) ;
#2329 = EDGE_CURVE ( 'NONE', #3476, #5356, #7236, .T. ) ;
#2330 = EDGE_CURVE ( 'NONE', #4907, #6616, #2130, .T. ) ;
#2331 = DIRECTION ( 'NONE',  ( 0.6157549048526804736, -0.7879377495398138809, -0.000000000000000000 ) ) ;
#2332 = ORIENTED_EDGE ( 'NONE', *, *, #5031, .T. ) ;
#2333 = DIRECTION ( 'NONE',  ( 0.000000000000000000, 0.000000000000000000, 1.000000000000000000 ) ) ;
#2334 = CC_DESIGN_DATE_AND_TIME_ASSIGNMENT ( #96, #1437, ( #187 ) ) ;
#2335 = EDGE_CURVE ( 'NONE', #1300, #6, #3934, .T. ) ;
#2336 = FACE_BOUND ( 'NONE', #7313, .T. ) ;
#2337 = DIRECTION ( 'NONE',  ( -4.440892098500626162E-15, 0.000000000000000000, 1.000000000000000000 ) ) ;
#2338 = CALENDAR_DATE ( 2026, 9, 10 ) ;
#2339 = ORIENTED_EDGE ( 'NONE', *, *, #3925, .T. ) ;
#2340 = DIRECTION ( 'NONE',  ( -0.000000000000000000, -0.000000000000000000, -1.000000000000000000 ) ) ;
#2341 = DIRECTION ( 'NONE',  ( 0.000000000000000000, 0.000000000000000000, 1.000000000000000000 ) ) ;
#2342 = CARTESIAN_POINT ( 'NONE',  ( 3.690413561029368683, -8.374393170229348371, 0.1849999999999999978 ) ) ;
#2343 = VERTEX_POINT ( 'NONE', #6970 ) ;
#2344 = VERTEX_POINT ( 'NONE', #7618 ) ;
#2345 = CARTESIAN_POINT ( 'NONE',  ( 1.082008577330675347, 0.9412886604525910750, -0.3750000000000000555 ) ) ;
#2346 = CARTESIAN_POINT ( 'NONE',  ( 0.05834656284656428160, -0.4630751787972929856, 0.2365186885590826738 ) ) ;
#2347 = COORDINATED_UNIVERSAL_TIME_OFFSET ( 0, 0, .AHEAD. ) ;
#2348 = DIRECTION ( 'NONE',  ( -0.6157549048526801405, 0.7879377495398142139, 0.000000000000000000 ) ) ;
#2349 = DIRECTION ( 'NONE',  ( -1.000000000000000000, 0.000000000000000000, 0.000000000000000000 ) ) ;
#2350 = CARTESIAN_POINT ( 'NONE',  ( 6.067386035484807039, 0.2407470087491024868, 0.1849999999999999978 ) ) ;
#2351 = DATE_AND_TIME ( #5476, #3571 ) ;
#2352 = CYLINDRICAL_SURFACE ( 'NONE', #5196, 0.3547681700190749576 ) ;
#2353 = CARTESIAN_POINT ( 'NONE',  ( 0.03125000000000000000, 0.03125000000000000000, -0.1204106507132265275 ) ) ;
#2354 = VERTEX_POINT ( 'NONE', #5163 ) ;
#2355 = CARTESIAN_POINT ( 'NONE',  ( 1.568372102291784920, 1.166559938944232488, 0.1823255903230677766 ) ) ;
#2356 = DIRECTION ( 'NONE',  ( -1.000000000000000000, 0.000000000000000000, 0.000000000000000000 ) ) ;
#2357 = CARTESIAN_POINT ( 'NONE',  ( 1.278468178838435554, 1.054204894368677481, -0.03540237178041887034 ) ) ;
#2358 = CARTESIAN_POINT ( 'NONE',  ( 0.1250000000000000278, -0.03125000000000000000, 0.000000000000000000 ) ) ;
#2359 = ORIENTED_EDGE ( 'NONE', *, *, #7480, .F. ) ;
#2360 = CARTESIAN_POINT ( 'NONE',  ( 1.718286774861130795, 1.296381967182311135, 0.1842501703447952666 ) ) ;
#2361 = APPLICATION_CONTEXT ( 'configuration controlled 3d designs of mechanical parts and assemblies' ) ;
#2362 = EDGE_CURVE ( 'NONE', #6459, #5362, #6060, .T. ) ;
#2363 = EDGE_CURVE ( 'NONE', #6856, #365, #6712, .T. ) ;
#2364 = CARTESIAN_POINT ( 'NONE',  ( 0.000000000000000000, 0.000000000000000000, 0.000000000000000000 ) ) ;
#2365 = CARTESIAN_POINT ( 'NONE',  ( 6.191327929239392347, 0.4578608198540764507, -0.1250000000000000000 ) ) ;
#2366 = APPLICATION_PROTOCOL_DEFINITION ( 'international standard', 'config_control_design', 1994, #7559 ) ;
#2367 = ORIENTED_EDGE ( 'NONE', *, *, #4246, .T. ) ;
#2368 = CARTESIAN_POINT ( 'NONE',  ( 1.537918127343594454, 1.852987194258524983, 0.000000000000000000 ) ) ;
#2369 = FACE_OUTER_BOUND ( 'NONE', #1174, .T. ) ;
#2370 = ORIENTED_EDGE ( 'NONE', *, *, #857, .T. ) ;
#2371 = PLANE ( 'NONE',  #7366 ) ;
#2372 = EDGE_CURVE ( 'NONE', #225, #4105, #7664, .T. ) ;
#2373 = CIRCLE ( 'NONE', #1980, 0.3045082206899650812 ) ;
#2374 = EDGE_CURVE ( 'NONE', #4226, #5921, #4439, .T. ) ;
#2375 = EDGE_LOOP ( 'NONE', ( #4312, #2427, #5262, #5637 ) ) ;
#2376 = VECTOR ( 'NONE', #4704, 39.37007874015748143 ) ;
#2377 = DIRECTION ( 'NONE',  ( -0.000000000000000000, -0.000000000000000000, -1.000000000000000000 ) ) ;
#2378 = EDGE_LOOP ( 'NONE', ( #645, #2233 ) ) ;
#2379 = CARTESIAN_POINT ( 'NONE',  ( 0.000000000000000000, -0.03125000000000000000, 0.000000000000000000 ) ) ;
#2380 = APPROVAL_ROLE ( '' ) ;
#2381 = APPROVAL ( #4326, 'UNSPECIFIED' ) ;
#2382 = LINE ( 'NONE', #1697, #2170 ) ;
#2383 = EDGE_CURVE ( 'NONE', #3462, #2354, #2149, .T. ) ;
#2384 = AXIS2_PLACEMENT_3D ( 'NONE', #2003, #4470, #7711 ) ;
#2385 = ADVANCED_BREP_SHAPE_REPRESENTATION ( '', ( #6445, #6285, #3555 ), #5783 ) ;
#2386 = ORIENTED_EDGE ( 'NONE', *, *, #1078, .T. ) ;
#2387 = CARTESIAN_POINT ( 'NONE',  ( 0.3566525292043903339, -0.3408511508279103985, 0.2500000000000000000 ) ) ;
#2388 = DIRECTION ( 'NONE',  ( 0.000000000000000000, 0.000000000000000000, 1.000000000000000000 ) ) ;
#2389 = VECTOR ( 'NONE', #3654, 39.37007874015748143 ) ;
#2390 = DIRECTION ( 'NONE',  ( -0.7540216022612866720, -0.6568496200222103676, 0.000000000000000000 ) ) ;
#2391 = DATE_TIME_ROLE ( 'classification_date' ) ;
#2392 = CARTESIAN_POINT ( 'NONE',  ( -1.555749437692314885, 0.7037162015503708457, -0.1657613293278376587 ) ) ;
#2393 = CARTESIAN_POINT ( 'NONE',  ( 1.558102590443268154, 1.816567841683527584, -0.02494716445955213677 ) ) ;
#2394 = ORIENTED_EDGE ( 'NONE', *, *, #780, .T. ) ;
#2395 = CARTESIAN_POINT ( 'NONE',  ( 0.1210307295689817542, 0.6124999999999999334, 0.03125000000000000000 ) ) ;
#2396 = DIRECTION ( 'NONE',  ( 0.9987955914953421388, 0.04906492035527377366, -0.000000000000000000 ) ) ;
#2397 = AXIS2_PLACEMENT_3D ( 'NONE', #1122, #539, #7909 ) ;
#2398 = EDGE_LOOP ( 'NONE', ( #7164, #4495, #1516, #4412 ) ) ;
#2399 = CARTESIAN_POINT ( 'NONE',  ( 0.1250000000000000000, 1.530808498934191509E-17, 0.2500000000000000000 ) ) ;
#2400 = DIRECTION ( 'NONE',  ( 0.6568496200222108117, 0.7540216022612861169, 0.000000000000000000 ) ) ;
#2401 = AXIS2_PLACEMENT_3D ( 'NONE', #4827, #2858, #7769 ) ;
#2402 = EDGE_LOOP ( 'NONE', ( #3975, #3049, #1705, #5273, #3366, #7456 ) ) ;
#2403 = CARTESIAN_POINT ( 'NONE',  ( 4.390472339057044593, -2.510390028880329805, 0.1250000000000000000 ) ) ;
#2404 = APPROVAL_PERSON_ORGANIZATION ( #4284, #5699, #1775 ) ;
#2405 = AXIS2_PLACEMENT_3D ( 'NONE', #7856, #494, #6604 ) ;
#2406 = CARTESIAN_POINT ( 'NONE',  ( -1.723766588794375387, 1.115324847714046497, -0.08100000000000007194 ) ) ;
#2407 = CARTESIAN_POINT ( 'NONE',  ( 1.598412416413206305, 1.292942227395209365, 0.2367065158496169941 ) ) ;
#2408 = APPROVAL_STATUS ( 'not_yet_approved' ) ;
#2409 = ORIENTED_EDGE ( 'NONE', *, *, #1936, .F. ) ;
#2410 = CARTESIAN_POINT ( 'NONE',  ( -1.803041671366327314, 1.104810305277056592, 0.1649762307749162715 ) ) ;
#2411 = DIRECTION ( 'NONE',  ( -1.821231995776175725E-16, -1.000000000000000000, 0.000000000000000000 ) ) ;
#2412 = VECTOR ( 'NONE', #6140, 39.37007874015748143 ) ;
#2413 = AXIS2_PLACEMENT_3D ( 'NONE', #2406, #3029, #6802 ) ;
#2414 = VERTEX_POINT ( 'NONE', #6932 ) ;
#2415 = DIRECTION ( 'NONE',  ( 1.000000000000000000, 0.000000000000000000, 0.000000000000000000 ) ) ;
#2416 = AXIS2_PLACEMENT_3D ( 'NONE', #4202, #3133, #1124 ) ;
#2417 = CARTESIAN_POINT ( 'NONE',  ( 0.1000000000000000472, -0.03125000000000000000, 0.06250000000000000000 ) ) ;
#2418 = LINE ( 'NONE', #7314, #6329 ) ;
#2419 = DIMENSIONAL_EXPONENTS ( 1.000000000000000000, 0.000000000000000000, 0.000000000000000000, 0.000000000000000000, 0.000000000000000000, 0.000000000000000000, 0.000000000000000000 ) ;
#2420 = ITEM_DEFINED_TRANSFORMATION ( 'NONE', 'NONE', #3562,  #3555 ) ;
#2421 = DIRECTION ( 'NONE',  ( 0.000000000000000000, 0.000000000000000000, -1.000000000000000000 ) ) ;
#2422 = EDGE_CURVE ( 'NONE', #4959, #3419, #1964, .T. ) ;
#2423 = EDGE_CURVE ( 'NONE', #5238, #5382, #3859, .T. ) ;
#2424 = VERTEX_POINT ( 'NONE', #6359 ) ;
#2425 = AXIS2_PLACEMENT_3D ( 'NONE', #6244, #7380, #1811 ) ;
#2426 = ADVANCED_FACE ( 'NONE', ( #4558 ), #2703, .F. ) ;
#2427 = ORIENTED_EDGE ( 'NONE', *, *, #412, .T. ) ;
#2428 = CIRCLE ( 'NONE', #2184, 0.2112499999999999933 ) ;
#2429 = EDGE_CURVE ( 'NONE', #4688, #2760, #4365, .T. ) ;
#2430 = ORIENTED_EDGE ( 'NONE', *, *, #1880, .F. ) ;
#2431 = ORIENTED_EDGE ( 'NONE', *, *, #2723, .F. ) ;
#2432 = EDGE_CURVE ( 'NONE', #5830, #4799, #1212, .T. ) ;
#2433 = CARTESIAN_POINT ( 'NONE',  ( 6.185915932927993133, 0.4597367884986663933, 0.1850000000000003586 ) ) ;
#2434 = VECTOR ( 'NONE', #947, 39.37007874015748143 ) ;
#2435 = LINE ( 'NONE', #3756, #5857 ) ;
#2436 = CARTESIAN_POINT ( 'NONE',  ( -0.02691317796861998624, -0.4609456947455670695, -2.734515813970577218E-17 ) ) ;
#2437 = COORDINATED_UNIVERSAL_TIME_OFFSET ( 0, 0, .AHEAD. ) ;
#2438 = CYLINDRICAL_SURFACE ( 'NONE', #5169, 0.3099999999999745737 ) ;
#2439 = ORIENTED_EDGE ( 'NONE', *, *, #1731, .F. ) ;
#2440 = VECTOR ( 'NONE', #6956, 39.37007874015748143 ) ;
#2441 = AXIS2_PLACEMENT_3D ( 'NONE', #3905, #6401, #3938 ) ;
#2442 = FACE_OUTER_BOUND ( 'NONE', #385, .T. ) ;
#2443 = VECTOR ( 'NONE', #7337, 39.37007874015748143 ) ;
#2444 = DIRECTION ( 'NONE',  ( -1.000000000000000000, 0.000000000000000000, 0.000000000000000000 ) ) ;
#2445 = CARTESIAN_POINT ( 'NONE',  ( 1.258616367985684104, -0.02482036785324303815, -0.1849999999999999978 ) ) ;
#2446 = DIRECTION ( 'NONE',  ( 0.7540216022612857838, -0.6568496200222112558, 7.922359181626369842E-15 ) ) ;
#2447 = ORIENTED_EDGE ( 'NONE', *, *, #22, .F. ) ;
#2448 = AXIS2_PLACEMENT_3D ( 'NONE', #3759, #716, #2474 ) ;
#2449 = LINE ( 'NONE', #6115, #3972 ) ;
#2450 = VECTOR ( 'NONE', #5456, 39.37007874015748854 ) ;
#2451 = ORIENTED_EDGE ( 'NONE', *, *, #4532, .T. ) ;
#2452 = DIRECTION ( 'NONE',  ( 0.000000000000000000, 1.000000000000000000, -0.000000000000000000 ) ) ;
#2453 = CARTESIAN_POINT ( 'NONE',  ( 1.733157827470031220, 1.373632878362992527, 0.1887011865795288901 ) ) ;
#2454 = PERSON_AND_ORGANIZATION ( #4735, #6190 ) ;
#2455 = VERTEX_POINT ( 'NONE', #4756 ) ;
#2456 = DIRECTION ( 'NONE',  ( 0.6568496200222109227, 0.7540216022612862279, 0.000000000000000000 ) ) ;
#2457 = EDGE_CURVE ( 'NONE', #6908, #140, #5870, .T. ) ;
#2458 = CARTESIAN_POINT ( 'NONE',  ( 0.9207653111462810180, 0.7459592875503607834, 0.03199999999999999373 ) ) ;
#2459 = ORIENTED_EDGE ( 'NONE', *, *, #2321, .F. ) ;
#2460 = DIRECTION ( 'NONE',  ( -0.2853335501257686646, 0.9584282785752022971, 0.000000000000000000 ) ) ;
#2461 = ORIENTED_EDGE ( 'NONE', *, *, #1281, .T. ) ;
#2462 = CYLINDRICAL_SURFACE ( 'NONE', #1013, 8.696493751522730520 ) ;
#2463 = DIRECTION ( 'NONE',  ( 0.7879377495398138809, 0.6157549048526804736, 0.000000000000000000 ) ) ;
#2464 = DATE_AND_TIME ( #8074, #6998 ) ;
#2465 = CARTESIAN_POINT ( 'NONE',  ( -0.6495791112554195612, -0.6379566159512914947, 0.2500000000000000000 ) ) ;
#2466 = EDGE_CURVE ( 'NONE', #4072, #353, #3525, .T. ) ;
#2467 = ADVANCED_FACE ( 'NONE', ( #6601, #949 ), #248, .F. ) ;
#2468 = ADVANCED_FACE ( 'NONE', ( #4140 ), #7821, .F. ) ;
#2469 = ORIENTED_EDGE ( 'NONE', *, *, #421, .F. ) ;
#2470 = LINE ( 'NONE', #544, #4652 ) ;
#2471 = FACE_OUTER_BOUND ( 'NONE', #2476, .T. ) ;
#2472 = CARTESIAN_POINT ( 'NONE',  ( 0.1009065958848031352, -0.4585303180291604996, 0.02870908699598821029 ) ) ;
#2473 = CALENDAR_DATE ( 2026, 9, 10 ) ;
#2474 = DIRECTION ( 'NONE',  ( 0.2323175946639494671, -0.9726399823210830631, 0.000000000000000000 ) ) ;
#2475 = CARTESIAN_POINT ( 'NONE',  ( 1.556400554713971651, 1.293514327272109687, 0.2500000000000000000 ) ) ;
#2476 = EDGE_LOOP ( 'NONE', ( #623, #5473, #7791, #5235 ) ) ;
#2477 = DIRECTION ( 'NONE',  ( -0.000000000000000000, -1.000000000000000000, -0.000000000000000000 ) ) ;
#2478 = CC_DESIGN_PERSON_AND_ORGANIZATION_ASSIGNMENT ( #1189, #3657, ( #7483 ) ) ;
#2479 = EDGE_CURVE ( 'NONE', #526, #5676, #2786, .T. ) ;
#2480 = ORIENTED_EDGE ( 'NONE', *, *, #2190, .T. ) ;
#2481 = CARTESIAN_POINT ( 'NONE',  ( 0.1250000000000000278, 0.03125000000000000000, 0.06250000000000000000 ) ) ;
#2482 = CARTESIAN_POINT ( 'NONE',  ( 1.340393471235059142, 1.071778002415290754, -0.1053413153387159629 ) ) ;
#2483 = CC_DESIGN_PERSON_AND_ORGANIZATION_ASSIGNMENT ( #1521, #1563, ( #4083 ) ) ;
#2484 = CARTESIAN_POINT ( 'NONE',  ( 1.790638542569023439, 1.445778985265036010, 0.1291092984545429978 ) ) ;
#2485 = ORIENTED_EDGE ( 'NONE', *, *, #1829, .T. ) ;
#2486 = CARTESIAN_POINT ( 'NONE',  ( 6.213241126991893459, 0.5142750483228205605, 0.1850000000000003586 ) ) ;
#2487 = VERTEX_POINT ( 'NONE', #2216 ) ;
#2488 = CARTESIAN_POINT ( 'NONE',  ( 1.723083782078303594, 1.395997476763640277, 0.1965221205737707477 ) ) ;
#2489 = FACE_OUTER_BOUND ( 'NONE', #6202, .T. ) ;
#2490 = COORDINATED_UNIVERSAL_TIME_OFFSET ( 0, 0, .AHEAD. ) ;
#2491 = ORIENTED_EDGE ( 'NONE', *, *, #899, .F. ) ;
#2492 = LINE ( 'NONE', #5000, #7173 ) ;
#2493 = DIRECTION ( 'NONE',  ( -0.000000000000000000, -1.000000000000000000, -0.000000000000000000 ) ) ;
#2494 = ORIENTED_EDGE ( 'NONE', *, *, #6589, .F. ) ;
#2495 = FACE_BOUND ( 'NONE', #6376, .T. ) ;
#2496 = CC_DESIGN_APPROVAL ( #6496, ( #6959 ) ) ;
#2497 = ORIENTED_EDGE ( 'NONE', *, *, #2080, .F. ) ;
#2498 = LINE ( 'NONE', #4969, #7676 ) ;
#2499 = LENGTH_MEASURE_WITH_UNIT ( LENGTH_MEASURE( 0.02539999999999999897 ), #2006 );
#2500 = CARTESIAN_POINT ( 'NONE',  ( 1.412217567875231783, 1.057196047309451492, -0.1989038500118037456 ) ) ;
#2501 = DATE_TIME_ROLE ( 'classification_date' ) ;
#2502 = CARTESIAN_POINT ( 'NONE',  ( -1.050138139902704104, -0.7221301030214424266, 0.2500000000000000000 ) ) ;
#2503 = APPROVAL_PERSON_ORGANIZATION ( #3073, #2132, #4760 ) ;
#2504 = ORIENTED_EDGE ( 'NONE', *, *, #6683, .F. ) ;
#2505 = SHAPE_REPRESENTATION ( 'Cleco, Handle, Pivoting', ( #3555 ), #2249 ) ;
#2506 = VECTOR ( 'NONE', #4334, 39.37007874015748143 ) ;
#2507 = VERTEX_POINT ( 'NONE', #7210 ) ;
#2508 = LOCAL_TIME ( 14, 45, 32.00000000000000000, #3123 ) ;
#2509 = CYLINDRICAL_SURFACE ( 'NONE', #8032, 0.1250000000000000000 ) ;
#2510 = FACE_OUTER_BOUND ( 'NONE', #7662, .T. ) ;
#2511 = PERSON_AND_ORGANIZATION_ROLE ( 'creator' ) ;
#2512 = CARTESIAN_POINT ( 'NONE',  ( 1.258671604940865274, -0.02501003737716508274, 0.1850000000000003586 ) ) ;
#2513 = CARTESIAN_POINT ( 'NONE',  ( 6.190221022838899856, 0.4584861219976859026, 0.1850000000000003586 ) ) ;
#2514 = CIRCLE ( 'NONE', #3310, 0.06199999999999999956 ) ;
#2515 = ORIENTED_EDGE ( 'NONE', *, *, #5131, .F. ) ;
#2516 = CC_DESIGN_APPROVAL ( #424, ( #5404 ) ) ;
#2517 = CC_DESIGN_APPROVAL ( #2381, ( #7233 ) ) ;
#2518 = APPLICATION_CONTEXT ( 'configuration controlled 3d designs of mechanical parts and assemblies' ) ;
#2519 = EDGE_LOOP ( 'NONE', ( #7087, #1713, #5517, #7252 ) ) ;
#2520 = DIRECTION ( 'NONE',  ( 0.7540216022612863389, -0.6568496200222107007, 0.000000000000000000 ) ) ;
#2521 = EDGE_CURVE ( 'NONE', #3224, #4959, #7088, .T. ) ;
#2522 = CARTESIAN_POINT ( 'NONE',  ( 1.388552349919598194, 1.071937153724873859, -0.1822035261336616696 ) ) ;
#2523 = CARTESIAN_POINT ( 'NONE',  ( 1.850068364776406682, 1.494658567734585608, 0.000000000000000000 ) ) ;
#2524 = EDGE_CURVE ( 'NONE', #1061, #2657, #6973, .T. ) ;
#2525 = ORIENTED_EDGE ( 'NONE', *, *, #872, .T. ) ;
#2526 = AXIS2_PLACEMENT_3D ( 'NONE', #1140, #3021, #1793 ) ;
#2527 = CARTESIAN_POINT ( 'NONE',  ( 1.475891671935536609, 0.7226544316391472211, 0.1850000000000003586 ) ) ;
#2528 = EDGE_CURVE ( 'NONE', #91, #7381, #5804, .T. ) ;
#2529 = ORIENTED_EDGE ( 'NONE', *, *, #1569, .T. ) ;
#2530 = DIMENSIONAL_EXPONENTS ( 1.000000000000000000, 0.000000000000000000, 0.000000000000000000, 0.000000000000000000, 0.000000000000000000, 0.000000000000000000, 0.000000000000000000 ) ;
#2531 = CC_DESIGN_PERSON_AND_ORGANIZATION_ASSIGNMENT ( #4979, #1248, ( #7594 ) ) ;
#2532 = VECTOR ( 'NONE', #3467, 39.37007874015748143 ) ;
#2533 = EDGE_CURVE ( 'NONE', #7143, #6082, #3484, .T. ) ;
#2534 = VECTOR ( 'NONE', #3549, 39.37007874015748143 ) ;
#2535 = DIRECTION ( 'NONE',  ( -0.000000000000000000, -0.000000000000000000, -1.000000000000000000 ) ) ;
#2536 = LINE ( 'NONE', #859, #5584 ) ;
#2537 = DATE_AND_TIME ( #37, #6699 ) ;
#2538 = ORIENTED_EDGE ( 'NONE', *, *, #732, .F. ) ;
#2539 = DIRECTION ( 'NONE',  ( 0.2873478855663425535, -0.000000000000000000, 0.9578262852211522071 ) ) ;
#2540 = DIRECTION ( 'NONE',  ( 0.000000000000000000, 1.000000000000000000, 0.000000000000000000 ) ) ;
#2541 = DIRECTION ( 'NONE',  ( 0.7879377495398137699, 0.6157549048526805846, 0.000000000000000000 ) ) ;
#2542 = APPROVAL_PERSON_ORGANIZATION ( #7348, #7299, #2380 ) ;
#2543 = CIRCLE ( 'NONE', #7128, 0.01652128394798136474 ) ;
#2544 = FACE_OUTER_BOUND ( 'NONE', #5367, .T. ) ;
#2545 = CIRCLE ( 'NONE', #3602, 0.06250000000000000000 ) ;
#2546 = DIRECTION ( 'NONE',  ( -0.9726399823210830631, -0.2323175946639496336, 0.000000000000000000 ) ) ;
#2547 = TOROIDAL_SURFACE ( 'NONE', #3336, 4.032000000000000917, 0.03200000000000000067 ) ;
#2548 = CONTEXT_DEPENDENT_SHAPE_REPRESENTATION ( #797, #2243 ) ;
#2549 = CARTESIAN_POINT ( 'NONE',  ( -6.110602001756019419, -1.404684638105634820, -0.05999999999999999778 ) ) ;
#2550 = AXIS2_PLACEMENT_3D ( 'NONE', #6333, #5843, #2069 ) ;
#2551 = CIRCLE ( 'NONE', #4912, 0.2425000000000000211 ) ;
#2552 = VERTEX_POINT ( 'NONE', #2746 ) ;
#2553 = ORIENTED_EDGE ( 'NONE', *, *, #3088, .T. ) ;
#2554 = LENGTH_MEASURE_WITH_UNIT ( LENGTH_MEASURE( 0.02539999999999999897 ), #3173 );
#2555 = DIRECTION ( 'NONE',  ( -1.000000000000000000, 0.000000000000000000, 0.000000000000000000 ) ) ;
#2556 = COORDINATED_UNIVERSAL_TIME_OFFSET ( 0, 0, .AHEAD. ) ;
#2557 = CARTESIAN_POINT ( 'NONE',  ( -1.723766588794375387, 1.115324847714046497, -0.2959999999999997078 ) ) ;
#2558 = PLANE ( 'NONE',  #5697 ) ;
#2559 = AXIS2_PLACEMENT_3D ( 'NONE', #7826, #1478, #4153 ) ;
#2560 = ORIENTED_EDGE ( 'NONE', *, *, #3480, .T. ) ;
#2561 = CIRCLE ( 'NONE', #2046, 0.1250000000000000000 ) ;
#2562 = SECURITY_CLASSIFICATION ( '', '', #7225 ) ;
#2563 = PLANE ( 'NONE',  #843 ) ;
#2564 = VERTEX_POINT ( 'NONE', #7742 ) ;
#2566 = FACE_OUTER_BOUND ( 'NONE', #3952, .T. ) ;
#2565 = AXIS2_PLACEMENT_3D ( 'NONE', #195, #6389, #3854 ) ;
#2567 = CARTESIAN_POINT ( 'NONE',  ( 0.7739487307887357170, -0.3852760516983189110, 0.000000000000000000 ) ) ;
#2568 = CARTESIAN_POINT ( 'NONE',  ( -1.432604426929670494, 0.8194101287839825609, 0.1250000000000000000 ) ) ;
#2569 = ORIENTED_EDGE ( 'NONE', *, *, #5838, .T. ) ;
#2570 = DIRECTION ( 'NONE',  ( 0.000000000000000000, 0.000000000000000000, 1.000000000000000000 ) ) ;
#2571 = CIRCLE ( 'NONE', #611, 0.06249999999999995143 ) ;
#2572 = ADVANCED_FACE ( 'NONE', ( #7135 ), #5411, .F. ) ;
#2573 = EDGE_CURVE ( 'NONE', #6542, #6342, #7244, .T. ) ;
#2574 = EDGE_CURVE ( 'NONE', #6082, #3897, #2131, .T. ) ;
#2575 = VERTEX_POINT ( 'NONE', #1633 ) ;
#2576 = CARTESIAN_POINT ( 'NONE',  ( -0.9142296270274463676, 0.5739542246721696106, 0.1250000000000000000 ) ) ;
#2577 = DIRECTION ( 'NONE',  ( -0.6157549048526804736, 0.7879377495398138809, 0.000000000000000000 ) ) ;
#2578 = DATE_AND_TIME ( #5704, #681 ) ;
#2579 = ORIENTED_EDGE ( 'NONE', *, *, #1581, .F. ) ;
#2580 = CARTESIAN_POINT ( 'NONE',  ( 0.000000000000000000, 1.050000000000000044, 0.000000000000000000 ) ) ;
#2581 = AXIS2_PLACEMENT_3D ( 'NONE', #1845, #3000, #5499 ) ;
#2582 = CIRCLE ( 'NONE', #7036, 0.01652128394798136474 ) ;
#2583 = CARTESIAN_POINT ( 'NONE',  ( 1.258616367985684104, -0.02482036785324303815, -0.1849999999999999978 ) ) ;
#2584 = CARTESIAN_POINT ( 'NONE',  ( -5.996547682996108186, -1.882193845889703843, 0.000000000000000000 ) ) ;
#2585 = APPROVAL ( #3506, 'UNKNOWN' ) ;
#2586 = EDGE_CURVE ( 'NONE', #6313, #2507, #2093, .T. ) ;
#2587 = EDGE_CURVE ( 'NONE', #577, #7415, #2726, .T. ) ;
#2588 = DIRECTION ( 'NONE',  ( -0.000000000000000000, -1.000000000000000000, -0.000000000000000000 ) ) ;
#2589 = CARTESIAN_POINT ( 'NONE',  ( -4.352122087710509568, -0.2377406176185900555, 0.4792670380269004049 ) ) ;
#2590 = FACE_OUTER_BOUND ( 'NONE', #304, .T. ) ;
#2591 = CARTESIAN_POINT ( 'NONE',  ( 0.000000000000000000, 1.362500000000000044, 0.000000000000000000 ) ) ;
#2592 = LINE ( 'NONE', #7064, #3985 ) ;
#2593 = APPROVAL_STATUS ( 'not_yet_approved' ) ;
#2594 = FACE_OUTER_BOUND ( 'NONE', #6978, .T. ) ;
#2595 = DIRECTION ( 'NONE',  ( 1.000000000000000000, 0.000000000000000000, 0.000000000000000000 ) ) ;
#2596 = ORIENTED_EDGE ( 'NONE', *, *, #1586, .T. ) ;
#2597 = FACE_OUTER_BOUND ( 'NONE', #7070, .T. ) ;
#2598 = ORIENTED_EDGE ( 'NONE', *, *, #1579, .F. ) ;
#2599 = CARTESIAN_POINT ( 'NONE',  ( 0.000000000000000000, 0.000000000000000000, 0.000000000000000000 ) ) ;
#2600 = DIRECTION ( 'NONE',  ( -0.000000000000000000, -0.000000000000000000, -1.000000000000000000 ) ) ;
#2601 = FACE_OUTER_BOUND ( 'NONE', #6415, .T. ) ;
#2602 = ORIENTED_EDGE ( 'NONE', *, *, #4851, .T. ) ;
#2603 = CARTESIAN_POINT ( 'NONE',  ( 1.833071640066518793, 1.461597232314661099, 0.07336022493874648498 ) ) ;
#2604 = CARTESIAN_POINT ( 'NONE',  ( 0.000000000000000000, 0.6124999999999999334, 0.000000000000000000 ) ) ;
#2605 = APPROVAL_DATE_TIME ( #117, #4341 ) ;
#2606 = VERTEX_POINT ( 'NONE', #447 ) ;
#2607 = DIRECTION ( 'NONE',  ( 0.000000000000000000, 0.000000000000000000, 1.000000000000000000 ) ) ;
#2608 = DIRECTION ( 'NONE',  ( 0.7879377495398124376, 0.6157549048526823610, -0.000000000000000000 ) ) ;
#2609 = ORIENTED_EDGE ( 'NONE', *, *, #3349, .F. ) ;
#2610 = CARTESIAN_POINT ( 'NONE',  ( -0.1250000000000000000, 0.000000000000000000, 0.2500000000000000000 ) ) ;
#2611 = EDGE_CURVE ( 'NONE', #7825, #3263, #7458, .T. ) ;
#2612 = EDGE_CURVE ( 'NONE', #7141, #7994, #4232, .T. ) ;
#2613 = DIRECTION ( 'NONE',  ( 0.000000000000000000, 0.000000000000000000, -1.000000000000000000 ) ) ;
#2614 = CARTESIAN_POINT ( 'NONE',  ( -4.333023248637945635, -0.2158163646391421386, 0.4417670380269021480 ) ) ;
#2615 = DIRECTION ( 'NONE',  ( 0.6157549048526803626, -0.7879377495398141029, 0.000000000000000000 ) ) ;
#2616 = ADVANCED_FACE ( 'NONE', ( #4305 ), #6674, .T. ) ;
#2617 = COORDINATED_UNIVERSAL_TIME_OFFSET ( 0, 0, .AHEAD. ) ;
#2618 = CARTESIAN_POINT ( 'NONE',  ( 1.240314151020239564, 1.658956310969643022, 0.2179999999999999993 ) ) ;
#2619 = DIRECTION ( 'NONE',  ( 0.000000000000000000, 1.000000000000000000, 0.000000000000000000 ) ) ;
#2620 = ORIENTED_EDGE ( 'NONE', *, *, #7827, .T. ) ;
#2621 = EDGE_CURVE ( 'NONE', #5902, #477, #3026, .T. ) ;
#2622 = ORIENTED_EDGE ( 'NONE', *, *, #5635, .F. ) ;
#2623 = ORIENTED_EDGE ( 'NONE', *, *, #2457, .T. ) ;
#2624 = CC_DESIGN_PERSON_AND_ORGANIZATION_ASSIGNMENT ( #6300, #4566, ( #2761 ) ) ;
#2625 = ADVANCED_FACE ( 'NONE', ( #1840, #5526 ), #6801, .T. ) ;
#2626 = SHAPE_REPRESENTATION_RELATIONSHIP ( 'NONE' , 'NONE' ,  #2, #2385 ) ;
#2627 = B_SPLINE_CURVE_WITH_KNOTS ( 'NONE', 3,
 ( #606, #5691, #70, #4461, #2484, #1217, #7001, #3725, #3808, #2523 ),
 .UNSPECIFIED., .F., .F.,
 ( 4, 2, 2, 2, 4 ),
 ( 1.944054687082719846E-15, 0.001638661185932331404, 0.003277322371862718617, 0.004915983557793104745, 0.006554644743723490874 ),
 .UNSPECIFIED. ) ;
#2628 = DIRECTION ( 'NONE',  ( 0.7879377495398141029, 0.6157549048526801405, 0.000000000000000000 ) ) ;
#2629 = PERSON_AND_ORGANIZATION ( #4735, #6190 ) ;
#2630 = CARTESIAN_POINT ( 'NONE',  ( 1.594233409951963720, 1.779210072867621673, -0.05526284733805063992 ) ) ;
#2631 = CARTESIAN_POINT ( 'NONE',  ( -1.275477614966805673, 0.03477957369036089458, 0.000000000000000000 ) ) ;
#2632 = ORIENTED_EDGE ( 'NONE', *, *, #3093, .T. ) ;
#2633 = EDGE_LOOP ( 'NONE', ( #1547, #7969, #1391, #1750 ) ) ;
#2634 = CC_DESIGN_APPROVAL ( #2132, ( #3550 ) ) ;
#2635 = ORIENTED_EDGE ( 'NONE', *, *, #3873, .F. ) ;
#2636 = ORIENTED_EDGE ( 'NONE', *, *, #3148, .F. ) ;
#2637 = DIRECTION ( 'NONE',  ( 0.7879377495398138809, 0.6157549048526802515, 0.000000000000000000 ) ) ;
#2638 = VERTEX_POINT ( 'NONE', #527 ) ;
#2639 = CIRCLE ( 'NONE', #5790, 0.1875000000000000278 ) ;
#2640 = DIRECTION ( 'NONE',  ( 0.000000000000000000, 0.000000000000000000, 1.000000000000000000 ) ) ;
#2641 = DIRECTION ( 'NONE',  ( -0.000000000000000000, -0.000000000000000000, -1.000000000000000000 ) ) ;
#2642 = AXIS2_PLACEMENT_3D ( 'NONE', #5170, #5780, #1279 ) ;
#2643 = CARTESIAN_POINT ( 'NONE',  ( -1.723766588794375387, 1.115324847714046497, -0.08100000000000007194 ) ) ;
#2644 = DIRECTION ( 'NONE',  ( -0.000000000000000000, 0.000000000000000000, 1.000000000000000000 ) ) ;
#2645 = AXIS2_PLACEMENT_3D ( 'NONE', #7950, #4277, #6810 ) ;
#2646 = ORIENTED_EDGE ( 'NONE', *, *, #6845, .F. ) ;
#2647 = EDGE_CURVE ( 'NONE', #158, #1448, #6188, .T. ) ;
#2648 = CARTESIAN_POINT ( 'NONE',  ( 1.814546527701561329, 1.464390739155001953, 0.09167169929298568665 ) ) ;
#2649 = LINE ( 'NONE', #2087, #4801 ) ;
#2650 = DATE_AND_TIME ( #4626, #1982 ) ;
#2651 = DIRECTION ( 'NONE',  ( -0.000000000000000000, -0.000000000000000000, 1.000000000000000000 ) ) ;
#2652 = AXIS2_PLACEMENT_3D ( 'NONE', #2081, #7172, #1554 ) ;
#2653 = LINE ( 'NONE', #5159, #7284 ) ;
#2654 = CARTESIAN_POINT ( 'NONE',  ( -1.199609308151822873, -0.2200601767247205021, 0.2460795971987651820 ) ) ;
#2655 = EDGE_LOOP ( 'NONE', ( #6409, #352, #1306, #2560, #5999, #2451 ) ) ;
#2656 = DIRECTION ( 'NONE',  ( -0.000000000000000000, -1.000000000000000000, -0.000000000000000000 ) ) ;
#2657 = VERTEX_POINT ( 'NONE', #4839 ) ;
#2658 = VECTOR ( 'NONE', #3629, 39.37007874015748143 ) ;
#2659 = EDGE_CURVE ( 'NONE', #4174, #4226, #7973, .T. ) ;
#2660 = LINE ( 'NONE', #249, #3860 ) ;
#2661 = CARTESIAN_POINT ( 'NONE',  ( 0.000000000000000000, 0.000000000000000000, 0.1250000000000000000 ) ) ;
#2662 = DIRECTION ( 'NONE',  ( -0.9027647548387306431, 0.4301346270889693235, -9.685622369408956771E-19 ) ) ;
#2663 = PLANE ( 'NONE',  #4771 ) ;
#2664 = CARTESIAN_POINT ( 'NONE',  ( 0.2976660692273690456, -0.3850326757561704505, 0.2500000000000000000 ) ) ;
#2665 = AXIS2_PLACEMENT_3D ( 'NONE', #4739, #7237, #4206 ) ;
#2666 = CARTESIAN_POINT ( 'NONE',  ( -1.194903880989551359, -0.2358655892081394090, 0.000000000000000000 ) ) ;
#2667 = DATE_AND_TIME ( #1886, #2508 ) ;
#2668 = DIRECTION ( 'NONE',  ( -1.000000000000000000, 0.000000000000000000, 0.000000000000000000 ) ) ;
#2669 = EDGE_CURVE ( 'NONE', #880, #2236, #7506, .T. ) ;
#2670 = ORIENTED_EDGE ( 'NONE', *, *, #6942, .F. ) ;
#2671 = EDGE_CURVE ( 'NONE', #1856, #3378, #4492, .T. ) ;
#2672 = CARTESIAN_POINT ( 'NONE',  ( 1.475891671935536609, 0.7226544316391472211, -0.09375000000000005551 ) ) ;
#2673 = APPROVAL_DATE_TIME ( #5841, #4742 ) ;
#2674 = CARTESIAN_POINT ( 'NONE',  ( 0.000000000000000000, 0.000000000000000000, 0.000000000000000000 ) ) ;
#2675 = DIRECTION ( 'NONE',  ( 0.000000000000000000, 0.000000000000000000, 1.000000000000000000 ) ) ;
#2676 = ORIENTED_EDGE ( 'NONE', *, *, #1126, .T. ) ;
#2677 = CIRCLE ( 'NONE', #6613, 0.1250000000000000000 ) ;
#2678 = VECTOR ( 'NONE', #6883, 39.37007874015748143 ) ;
#2679 = EDGE_CURVE ( 'NONE', #3298, #2215, #2449, .T. ) ;
#2680 = EDGE_CURVE ( 'NONE', #2343, #2766, #3445, .T. ) ;
#2681 = EDGE_LOOP ( 'NONE', ( #5503, #4729, #724 ) ) ;
#2682 = DIRECTION ( 'NONE',  ( -0.07966912593697395018, 0.06940203694730379125, -0.9944024274105548455 ) ) ;
#2683 = VECTOR ( 'NONE', #3914, 39.37007874015748143 ) ;
#2684 = VERTEX_POINT ( 'NONE', #5573 ) ;
#2685 = CARTESIAN_POINT ( 'NONE',  ( 1.623596292979297528, 1.309516105093665228, 0.2332408580811136944 ) ) ;
#2686 = CARTESIAN_POINT ( 'NONE',  ( -0.03125000000000000000, 0.03125000000000000000, -0.1204106507132265275 ) ) ;
#2687 = CARTESIAN_POINT ( 'NONE',  ( 0.1250000000000000278, 0.03125000000000000000, 0.000000000000000000 ) ) ;
#2688 = ORIENTED_EDGE ( 'NONE', *, *, #5123, .T. ) ;
#2689 = CARTESIAN_POINT ( 'NONE',  ( 1.821662113731687560E-17, 1.393749999999999822, -0.1487499999999999933 ) ) ;
#2690 = VECTOR ( 'NONE', #7615, 39.37007874015748143 ) ;
#2691 = EDGE_LOOP ( 'NONE', ( #1153, #8022, #1054, #2224 ) ) ;
#2692 = CIRCLE ( 'NONE', #2836, 0.03200000000000003536 ) ;
#2693 = CIRCLE ( 'NONE', #1525, 0.2499400561648078278 ) ;
#2694 = CARTESIAN_POINT ( 'NONE',  ( 1.420131823442061014, 1.799479612255304284, 0.1337826180019923150 ) ) ;
#2695 = CARTESIAN_POINT ( 'NONE',  ( 0.000000000000000000, 0.03125000000000000000, -0.1487499999999999933 ) ) ;
#2696 = AXIS2_PLACEMENT_3D ( 'NONE', #6798, #7329, #2988 ) ;
#2697 = PERSON_AND_ORGANIZATION_ROLE ( 'creator' ) ;
#2698 = VERTEX_POINT ( 'NONE', #7332 ) ;
#2699 = FACE_OUTER_BOUND ( 'NONE', #4927, .T. ) ;
#2700 = FACE_OUTER_BOUND ( 'NONE', #5036, .T. ) ;
#2701 = ORIENTED_EDGE ( 'NONE', *, *, #8086, .T. ) ;
#2702 = AXIS2_PLACEMENT_3D ( 'NONE', #3468, #2240, #7880 ) ;
#2703 = PLANE ( 'NONE',  #1606 ) ;
#2704 = AXIS2_PLACEMENT_3D ( 'NONE', #1165, #7319, #3051 ) ;
#2705 = FACE_OUTER_BOUND ( 'NONE', #7695, .T. ) ;
#2706 = AXIS2_PLACEMENT_3D ( 'NONE', #615, #5532, #6724 ) ;
#2707 = DIRECTION ( 'NONE',  ( -0.6568496200222107007, -0.7540216022612862279, 0.000000000000000000 ) ) ;
#2708 = CALENDAR_DATE ( 2026, 9, 10 ) ;
#2709 = ORIENTED_EDGE ( 'NONE', *, *, #7281, .F. ) ;
#2710 = DIRECTION ( 'NONE',  ( -0.000000000000000000, -0.000000000000000000, 1.000000000000000000 ) ) ;
#2711 = CARTESIAN_POINT ( 'NONE',  ( 0.1000000000000000472, -0.03125000000000000000, 0.7124999999999989120 ) ) ;
#2712 = CIRCLE ( 'NONE', #2063, 0.03125000000000000694 ) ;
#2713 = VECTOR ( 'NONE', #2807, 39.37007874015748143 ) ;
#2714 = ORIENTED_EDGE ( 'NONE', *, *, #2986, .T. ) ;
#2715 = CARTESIAN_POINT ( 'NONE',  ( 0.000000000000000000, 0.000000000000000000, 0.000000000000000000 ) ) ;
#2716 = CARTESIAN_POINT ( 'NONE',  ( -0.6495791112554195612, -0.6379566159512914947, 0.03199999999999999373 ) ) ;
#2717 = LINE ( 'NONE', #5228, #1805 ) ;
#2718 = COORDINATED_UNIVERSAL_TIME_OFFSET ( 0, 0, .AHEAD. ) ;
#2719 = CARTESIAN_POINT ( 'NONE',  ( 0.000000000000000000, 0.000000000000000000, 0.09374999999999998612 ) ) ;
#2720 = CARTESIAN_POINT ( 'NONE',  ( 3.690413561029368683, -8.374393170229348371, 0.1849999999999999978 ) ) ;
#2721 = ORIENTED_EDGE ( 'NONE', *, *, #4533, .T. ) ;
#2722 = EDGE_LOOP ( 'NONE', ( #1770, #905, #839, #6019 ) ) ;
#2723 = EDGE_CURVE ( 'NONE', #1929, #6526, #4918, .T. ) ;
#2724 = ADVANCED_FACE ( 'NONE', ( #6235 ), #1714, .F. ) ;
#2725 = EDGE_CURVE ( 'NONE', #2564, #6669, #1354, .T. ) ;
#2726 = B_SPLINE_CURVE_WITH_KNOTS ( 'NONE', 3,
 ( #6533, #918, #7783, #2178, #4676, #3444 ),
 .UNSPECIFIED., .F., .F.,
 ( 4, 2, 4 ),
 ( 0.002381428155045459648, 0.003857366089970378029, 0.005333304024895296411 ),
 .UNSPECIFIED. ) ;
#2727 = ORIENTED_EDGE ( 'NONE', *, *, #2647, .F. ) ;
#2728 = ORIENTED_EDGE ( 'NONE', *, *, #5354, .F. ) ;
#2729 = CARTESIAN_POINT ( 'NONE',  ( 0.000000000000000000, -0.03125000000000000000, 0.000000000000000000 ) ) ;
#2730 = ORIENTED_EDGE ( 'NONE', *, *, #7399, .T. ) ;
#2731 = CARTESIAN_POINT ( 'NONE',  ( 1.678550149446894624, 1.340866106857560247, 0.2177700924245533909 ) ) ;
#2732 = CARTESIAN_POINT ( 'NONE',  ( -0.04782642554762441683, -0.03125000000000000000, 0.07449999999999999678 ) ) ;
#2733 = CARTESIAN_POINT ( 'NONE',  ( 0.000000000000000000, 0.000000000000000000, 0.1250000000000000000 ) ) ;
#2734 = ORIENTED_EDGE ( 'NONE', *, *, #5540, .T. ) ;
#2735 = DIRECTION ( 'NONE',  ( 1.000000000000000000, 0.000000000000000000, 0.000000000000000000 ) ) ;
#2736 = EDGE_CURVE ( 'NONE', #3378, #4578, #828, .T. ) ;
#2737 = ORIENTED_EDGE ( 'NONE', *, *, #2887, .T. ) ;
#2738 = CARTESIAN_POINT ( 'NONE',  ( 1.301246111754461809, 1.706573211805008539, 0.2436449323019636015 ) ) ;
#2739 = APPROVAL ( #3970, 'UNSPECIFIED' ) ;
#2740 = CARTESIAN_POINT ( 'NONE',  ( 0.000000000000000000, 0.000000000000000000, -0.6219999999999999973 ) ) ;
#2741 = DATE_AND_TIME ( #243, #5006 ) ;
#2742 = EDGE_CURVE ( 'NONE', #4799, #1231, #39, .T. ) ;
#2743 = ORIENTED_EDGE ( 'NONE', *, *, #882, .F. ) ;
#2744 = CARTESIAN_POINT ( 'NONE',  ( -1.803041671366327314, 1.104810305277056592, 0.1649762307749162715 ) ) ;
#2745 = DIRECTION ( 'NONE',  ( 1.000000000000000000, 0.000000000000000000, 0.000000000000000000 ) ) ;
#2746 = CARTESIAN_POINT ( 'NONE',  ( 6.213241126991890795, 0.5142750483228147873, -0.1849999999999999978 ) ) ;
#2747 = DIRECTION ( 'NONE',  ( 0.000000000000000000, 0.000000000000000000, -1.000000000000000000 ) ) ;
#2748 = DIRECTION ( 'NONE',  ( 0.000000000000000000, 1.000000000000000000, 0.000000000000000000 ) ) ;
#2749 = APPLICATION_PROTOCOL_DEFINITION ( 'international standard', 'config_control_design', 1994, #3474 ) ;
#2750 = VERTEX_POINT ( 'NONE', #2527 ) ;
#2751 = DIRECTION ( 'NONE',  ( 0.6157549048526804736, -0.7879377495398138809, -0.000000000000000000 ) ) ;
#2752 = DIRECTION ( 'NONE',  ( 0.2815666759589948720, -0.9595416650617117904, 0.000000000000000000 ) ) ;
#2753 = EDGE_LOOP ( 'NONE', ( #2296, #2853, #6918, #2439, #2811 ) ) ;
#2754 = FACE_OUTER_BOUND ( 'NONE', #1102, .T. ) ;
#2755 = CYLINDRICAL_SURFACE ( 'NONE', #753, 7.490657474112464520 ) ;
#2756 = ITEM_DEFINED_TRANSFORMATION ( 'NONE', 'NONE', #7098,  #3555 ) ;
#2757 = DIRECTION ( 'NONE',  ( 1.000000000000000000, 0.000000000000000000, 0.000000000000000000 ) ) ;
#2758 = CYLINDRICAL_SURFACE ( 'NONE', #1904, 0.3024878104022636904 ) ;
#2759 = VERTEX_POINT ( 'NONE', #6278 ) ;
#2760 = VERTEX_POINT ( 'NONE', #5655 ) ;
#2761 = PRODUCT ( 'Cleco, Handle, Stationary', 'Cleco, Handle, Stationary', '', ( #56 ) ) ;
#2762 = ORIENTED_EDGE ( 'NONE', *, *, #2329, .F. ) ;
#2763 = ORIENTED_EDGE ( 'NONE', *, *, #1479, .F. ) ;
#2764 = CARTESIAN_POINT ( 'NONE',  ( 1.275565605498405253, -0.08258253728086821510, 5.393636709996481038 ) ) ;
#2765 = DESIGN_CONTEXT ( 'detailed design', #3474, 'design' ) ;
#2766 = VERTEX_POINT ( 'NONE', #2486 ) ;
#2767 = CARTESIAN_POINT ( 'NONE',  ( 1.620241226944308055, 1.319147010849713419, 0.2447046302806205054 ) ) ;
#2768 = DIRECTION ( 'NONE',  ( -0.7540216022612858948, 0.6568496200222110337, 0.000000000000000000 ) ) ;
#2769 = DIRECTION ( 'NONE',  ( -0.04906492035527430795, 0.9987955914953422498, 0.000000000000000000 ) ) ;
#2770 = ORIENTED_EDGE ( 'NONE', *, *, #2528, .T. ) ;
#2771 =( GEOMETRIC_REPRESENTATION_CONTEXT ( 3 ) GLOBAL_UNCERTAINTY_ASSIGNED_CONTEXT ( ( #975 ) ) GLOBAL_UNIT_ASSIGNED_CONTEXT ( ( #4074, #4653, #3502 ) ) REPRESENTATION_CONTEXT ( 'NONE', 'WORKASPACE' ) );
#2772 = DIRECTION ( 'NONE',  ( -0.7879377495398141029, -0.6157549048526800295, -0.000000000000000000 ) ) ;
#2773 = LOCAL_TIME ( 14, 45, 32.00000000000000000, #196 ) ;
#2774 = SHAPE_REPRESENTATION ( 'Cleco, Fastener, Center, Split', ( #3555 ), #2122 ) ;
#2775 = AXIS2_PLACEMENT_3D ( 'NONE', #1299, #3266, #5076 ) ;
#2776 = EDGE_LOOP ( 'NONE', ( #7850, #4571 ) ) ;
#2777 = CARTESIAN_POINT ( 'NONE',  ( 1.538653472941177380, 1.853533897300119637, -0.002614644835676915424 ) ) ;
#2778 = DIRECTION ( 'NONE',  ( 0.000000000000000000, 0.000000000000000000, -1.000000000000000000 ) ) ;
#2779 = APPLICATION_PROTOCOL_DEFINITION ( 'international standard', 'config_control_design', 1994, #3900 ) ;
#2780 = EDGE_CURVE ( 'NONE', #3425, #6917, #1301, .T. ) ;
#2781 = EDGE_CURVE ( 'NONE', #5923, #2970, #4547, .T. ) ;
#2782 = DIRECTION ( 'NONE',  ( 0.6157549048526803626, -0.7879377495398141029, 0.000000000000000000 ) ) ;
#2783 = CARTESIAN_POINT ( 'NONE',  ( 0.03125000000000000000, 0.000000000000000000, 0.1106726592253027830 ) ) ;
#2784 = ORIENTED_EDGE ( 'NONE', *, *, #2573, .F. ) ;
#2785 = ADVANCED_FACE ( 'NONE', ( #7045 ), #5695, .F. ) ;
#2786 = CIRCLE ( 'NONE', #3833, 0.1100000000000000006 ) ;
#2787 = ADVANCED_BREP_SHAPE_REPRESENTATION ( '', ( #6340, #3555 ), #1726 ) ;
#2788 = DIRECTION ( 'NONE',  ( -0.000000000000000000, -1.000000000000000000, -0.000000000000000000 ) ) ;
#2789 = APPROVAL ( #5317, 'UNKNOWN' ) ;
#2790 = ADVANCED_FACE ( 'NONE', ( #3773 ), #3192, .T. ) ;
#2791 = EDGE_CURVE ( 'NONE', #3779, #2877, #3181, .T. ) ;
#2792 = AXIS2_PLACEMENT_3D ( 'NONE', #6068, #7941, #2333 ) ;
#2793 = DIRECTION ( 'NONE',  ( -0.000000000000000000, -0.000000000000000000, 1.000000000000000000 ) ) ;
#2794 =( REPRESENTATION_RELATIONSHIP ('NONE','NONE', #3360, #2505 ) REPRESENTATION_RELATIONSHIP_WITH_TRANSFORMATION ( #2756 )SHAPE_REPRESENTATION_RELATIONSHIP( ) );
#2795 = CARTESIAN_POINT ( 'NONE',  ( -1.411633252941551619, 0.8434166392007494961, 0.1250000000000000000 ) ) ;
#2796 = MECHANICAL_CONTEXT ( 'NONE', #4728, 'mechanical' ) ;
#2797 = ORIENTED_EDGE ( 'NONE', *, *, #4786, .F. ) ;
#2798 = CARTESIAN_POINT ( 'NONE',  ( 1.640223930642815242, 1.235377681955144746, -0.1039999999999998703 ) ) ;
#2799 = CARTESIAN_POINT ( 'NONE',  ( 1.552534361087756443, 1.258070674485461060, 0.2367071595535535922 ) ) ;
#2800 = EDGE_LOOP ( 'NONE', ( #4552, #4510, #5467, #537 ) ) ;
#2801 = EDGE_CURVE ( 'NONE', #1645, #4391, #6312, .T. ) ;
#2802 = ORIENTED_EDGE ( 'NONE', *, *, #7496, .T. ) ;
#2803 = AXIS2_PLACEMENT_3D ( 'NONE', #1290, #3015, #2390 ) ;
#2804 = ORIENTED_EDGE ( 'NONE', *, *, #5901, .F. ) ;
#2805 = DIRECTION ( 'NONE',  ( 0.000000000000000000, 0.000000000000000000, -1.000000000000000000 ) ) ;
#2806 = CIRCLE ( 'NONE', #2011, 0.2148203157102362704 ) ;
#2807 = DIRECTION ( 'NONE',  ( 1.000000000000000000, 0.000000000000000000, 0.000000000000000000 ) ) ;
#2808 = APPROVAL_DATE_TIME ( #5360, #2585 ) ;
#2809 = CARTESIAN_POINT ( 'NONE',  ( 0.000000000000000000, 0.000000000000000000, 0.000000000000000000 ) ) ;
#2810 = ORIENTED_EDGE ( 'NONE', *, *, #7595, .F. ) ;
#2811 = ORIENTED_EDGE ( 'NONE', *, *, #2991, .F. ) ;
#2812 = CC_DESIGN_APPROVAL ( #7299, ( #1105 ) ) ;
#2813 = AXIS2_PLACEMENT_3D ( 'NONE', #288, #5871, #4065 ) ;
#2814 = PLANE ( 'NONE',  #6870 ) ;
#2815 = VERTEX_POINT ( 'NONE', #4477 ) ;
#2816 = FACE_BOUND ( 'NONE', #3524, .T. ) ;
#2817 = LINE ( 'NONE', #5975, #3632 ) ;
#2818 = AXIS2_PLACEMENT_3D ( 'NONE', #4830, #2273, #6100 ) ;
#2819 = AXIS2_PLACEMENT_3D ( 'NONE', #7976, #7375, #4805 ) ;
#2820 = DIRECTION ( 'NONE',  ( 0.000000000000000000, 0.000000000000000000, -1.000000000000000000 ) ) ;
#2821 = DIRECTION ( 'NONE',  ( 0.7879377495398141029, 0.6157549048526802515, 6.186071356164057065E-15 ) ) ;
#2822 = AXIS2_PLACEMENT_3D ( 'NONE', #3090, #2421, #6779 ) ;
#2823 = CARTESIAN_POINT ( 'NONE',  ( 0.000000000000000000, 1.081250000000000044, 0.000000000000000000 ) ) ;
#2824 = DIRECTION ( 'NONE',  ( -0.6568496200222107007, -0.7540216022612863389, 0.000000000000000000 ) ) ;
#2825 = DIRECTION ( 'NONE',  ( 0.000000000000000000, 0.000000000000000000, 1.000000000000000000 ) ) ;
#2826 = TOROIDAL_SURFACE ( 'NONE', #6495, 0.1255000000000000282, 0.06199999999999999956 ) ;
#2827 = VERTEX_POINT ( 'NONE', #7651 ) ;
#2828 = CARTESIAN_POINT ( 'NONE',  ( 0.000000000000000000, 0.000000000000000000, -0.5599999999999999423 ) ) ;
#2829 =( BOUNDED_SURFACE ( )  B_SPLINE_SURFACE ( 3, 2, ( 
 ( #4161, #6546, #6010 ),
 ( #1044, #4077, #2880 ),
 ( #7866, #967, #4199 ),
 ( #6040, #3421, #3387 ) ),
 .UNSPECIFIED., .F., .F., .T. ) 
 B_SPLINE_SURFACE_WITH_KNOTS ( ( 4, 4 ),
 ( 3, 3 ),
 ( 2.890916672715349023E-15, 0.001713611390987410501 ),
 ( 0.000000000000000000, 1.000000000000000000 ),
 .UNSPECIFIED. ) 
 GEOMETRIC_REPRESENTATION_ITEM ( )  RATIONAL_B_SPLINE_SURFACE ( (
 ( 1.000000000000000000, 0.7881701093123700819, 1.000000000000000000),
 ( 1.000000000000000000, 0.7634790912858369083, 1.000000000000000000),
 ( 1.000000000000000000, 0.7360895404014861088, 1.000000000000000000),
 ( 1.000000000000000000, 0.7071067811865471286, 1.000000000000000000) ) ) 
 REPRESENTATION_ITEM ( '' )  SURFACE ( )  );
#2830 = ADVANCED_FACE ( 'NONE', ( #3886, #1922 ), #3154, .T. ) ;
#2831 = ADVANCED_FACE ( 'NONE', ( #2601 ), #4431, .F. ) ;
#2832 = FACE_OUTER_BOUND ( 'NONE', #6572, .T. ) ;
#2833 = CARTESIAN_POINT ( 'NONE',  ( 1.417678740269246340, 1.200983045140381122, 0.2500000000000000000 ) ) ;
#2834 = PERSON_AND_ORGANIZATION ( #4735, #6190 ) ;
#2835 = EDGE_LOOP ( 'NONE', ( #1568, #7995, #4048, #2183 ) ) ;
#2836 = AXIS2_PLACEMENT_3D ( 'NONE', #7818, #4625, #7130 ) ;
#2837 = AXIS2_PLACEMENT_3D ( 'NONE', #5291, #2782, #7780 ) ;
#2838 = CARTESIAN_POINT ( 'NONE',  ( 1.492904096916551460, 1.856349440303736831, -0.001813861035895662039 ) ) ;
#2839 = PRODUCT_DEFINITION_SHAPE ( 'NONE', 'NONE',  #5402 ) ;
#2840 = CARTESIAN_POINT ( 'NONE',  ( 1.353740795342265546, 0.002292344206094486941, -0.1250000000000000000 ) ) ;
#2841 = ADVANCED_FACE ( 'NONE', ( #5077 ), #730, .T. ) ;
#2842 = VERTEX_POINT ( 'NONE', #4463 ) ;
#2843 = ORIENTED_EDGE ( 'NONE', *, *, #7592, .F. ) ;
#2844 = CIRCLE ( 'NONE', #3373, 0.03125000000000000000 ) ;
#2845 = ORIENTED_EDGE ( 'NONE', *, *, #1126, .F. ) ;
#2846 = SHAPE_REPRESENTATION_RELATIONSHIP ( 'NONE' , 'NONE' ,  #2505, #3861 ) ;
#2847 = ORIENTED_EDGE ( 'NONE', *, *, #80, .T. ) ;
#2848 = CARTESIAN_POINT ( 'NONE',  ( -0.1250000000000000000, 0.5625000000000000000, 0.03125000000000000000 ) ) ;
#2849 = CARTESIAN_POINT ( 'NONE',  ( -0.01467241879803482009, -0.4621469832361911889, 0.2490901869219590559 ) ) ;
#2850 = DATE_TIME_ROLE ( 'classification_date' ) ;
#2851 = CARTESIAN_POINT ( 'NONE',  ( 2.204364238465235822E-17, 1.112500000000000044, 0.1799999999999999933 ) ) ;
#2852 = CIRCLE ( 'NONE', #7031, 0.06199999999999999956 ) ;
#2853 = ORIENTED_EDGE ( 'NONE', *, *, #4636, .T. ) ;
#2854 = AXIS2_PLACEMENT_3D ( 'NONE', #7270, #7834, #5924 ) ;
#2855 = VERTEX_POINT ( 'NONE', #6958 ) ;
#2856 = DIRECTION ( 'NONE',  ( -0.6578909993250587895, -0.7531131608245040798, 0.000000000000000000 ) ) ;
#2857 = DESIGN_CONTEXT ( 'detailed design', #7659, 'design' ) ;
#2858 = DIRECTION ( 'NONE',  ( -0.6157549048526804736, 0.7879377495398138809, 0.000000000000000000 ) ) ;
#2859 = CARTESIAN_POINT ( 'NONE',  ( 0.000000000000000000, 0.000000000000000000, 0.06199999999999999956 ) ) ;
#2860 = ORIENTED_EDGE ( 'NONE', *, *, #376, .T. ) ;
#2861 = DIRECTION ( 'NONE',  ( 0.04906492035527378059, -0.9987955914953422498, 0.000000000000000000 ) ) ;
#2862 = CARTESIAN_POINT ( 'NONE',  ( -1.194903880989551359, -0.2358655892081394090, 0.2500000000000000000 ) ) ;
#2863 = ORIENTED_EDGE ( 'NONE', *, *, #522, .T. ) ;
#2864 = LINE ( 'NONE', #5939, #1113 ) ;
#2865 = DIRECTION ( 'NONE',  ( 0.000000000000000000, 0.000000000000000000, -1.000000000000000000 ) ) ;
#2866 = LINE ( 'NONE', #7892, #1518 ) ;
#2867 = ORIENTED_EDGE ( 'NONE', *, *, #2190, .F. ) ;
#2868 = CARTESIAN_POINT ( 'NONE',  ( 0.000000000000000000, 0.000000000000000000, 0.000000000000000000 ) ) ;
#2869 = CARTESIAN_POINT ( 'NONE',  ( -1.204376266962890796, -0.2040480809676099294, 0.02769383754956057653 ) ) ;
#2870 = CARTESIAN_POINT ( 'NONE',  ( 1.515234606834908515, 1.873800211025280271, -0.03184469952871944037 ) ) ;
#2871 = DATE_AND_TIME ( #2708, #2133 ) ;
#2872 = ORIENTED_EDGE ( 'NONE', *, *, #3533, .F. ) ;
#2873 = DIRECTION ( 'NONE',  ( -0.7879377495398137699, -0.6157549048526804736, 9.031266384036010773E-16 ) ) ;
#2874 = FACE_OUTER_BOUND ( 'NONE', #6890, .T. ) ;
#2875 = PERSON ( 'NAUO-PER5', 'UNSPECIFIED', 'UNSPECIFIED', ('UNSPECIFIED'), ('UNSPECIFIED'), ('UNSPECIFIED') ) ;
#2876 = ORIENTED_EDGE ( 'NONE', *, *, #469, .T. ) ;
#2877 = VERTEX_POINT ( 'NONE', #5109 ) ;
#2878 = ORIENTED_EDGE ( 'NONE', *, *, #6250, .F. ) ;
#2879 = DIRECTION ( 'NONE',  ( -0.000000000000000000, -1.000000000000000000, -0.000000000000000000 ) ) ;
#2880 = CARTESIAN_POINT ( 'NONE',  ( 1.434403980295607450, 1.174077354389669425, 0.2232676372131965070 ) ) ;
#2881 = COORDINATED_UNIVERSAL_TIME_OFFSET ( 0, 0, .AHEAD. ) ;
#2882 = CARTESIAN_POINT ( 'NONE',  ( 0.09537553527426689826, -0.4271221084841553828, 0.03199999999999999373 ) ) ;
#2883 = ADVANCED_FACE ( 'NONE', ( #1993 ), #6386, .T. ) ;
#2884 = ADVANCED_FACE ( 'NONE', ( #5769 ), #1878, .T. ) ;
#2885 = ADVANCED_FACE ( 'NONE', ( #6422 ), #804, .F. ) ;
#2886 = CC_DESIGN_DATE_AND_TIME_ASSIGNMENT ( #7082, #6704, ( #7247 ) ) ;
#2887 = EDGE_CURVE ( 'NONE', #2327, #4578, #6066, .T. ) ;
#2888 = CARTESIAN_POINT ( 'NONE',  ( 0.1250000000000000000, 0.5625000000000000000, 0.03125000000000000000 ) ) ;
#2889 = CARTESIAN_POINT ( 'NONE',  ( -0.5950975756886838219, 0.1840126700235215629, 0.000000000000000000 ) ) ;
#2890 = CARTESIAN_POINT ( 'NONE',  ( 1.353740795342265546, 0.002292344206094486941, -0.1250000000000000000 ) ) ;
#2891 = LINE ( 'NONE', #7922, #3469 ) ;
#2892 = EDGE_LOOP ( 'NONE', ( #462, #4178 ) ) ;
#2893 = DIRECTION ( 'NONE',  ( -0.7540216022612861169, 0.6568496200222109227, 0.000000000000000000 ) ) ;
#2894 = FACE_OUTER_BOUND ( 'NONE', #408, .T. ) ;
#2895 = VERTEX_POINT ( 'NONE', #1457 ) ;
#2896 = DIRECTION ( 'NONE',  ( -0.000000000000000000, -0.000000000000000000, -1.000000000000000000 ) ) ;
#2897 = DIRECTION ( 'NONE',  ( 0.000000000000000000, -0.000000000000000000, -1.000000000000000000 ) ) ;
#2898 = LOCAL_TIME ( 14, 45, 32.00000000000000000, #3528 ) ;
#2899 = CARTESIAN_POINT ( 'NONE',  ( 0.000000000000000000, 0.6124999999999999334, 0.000000000000000000 ) ) ;
#2900 = EDGE_LOOP ( 'NONE', ( #5351, #3384, #6718, #1542, #644, #7504 ) ) ;
#2901 = DIRECTION ( 'NONE',  ( 0.000000000000000000, 1.000000000000000000, 0.000000000000000000 ) ) ;
#2902 = AXIS2_PLACEMENT_3D ( 'NONE', #6020, #6790, #3643 ) ;
#2903 = LOCAL_TIME ( 14, 45, 32.00000000000000000, #2490 ) ;
#2904 = DIRECTION ( 'NONE',  ( -0.000000000000000000, -0.000000000000000000, -1.000000000000000000 ) ) ;
#2905 = DIRECTION ( 'NONE',  ( -1.000000000000000000, 0.000000000000000000, 0.000000000000000000 ) ) ;
#2906 = PERSON_AND_ORGANIZATION_ROLE ( 'creator' ) ;
#2907 = EDGE_LOOP ( 'NONE', ( #733, #6025, #4196, #2154 ) ) ;
#2908 = VECTOR ( 'NONE', #2116, 39.37007874015748143 ) ;
#2909 = DIRECTION ( 'NONE',  ( 0.000000000000000000, 0.000000000000000000, 1.000000000000000000 ) ) ;
#2910 = CARTESIAN_POINT ( 'NONE',  ( 0.000000000000000000, -0.03125000000000000000, 0.000000000000000000 ) ) ;
#2911 = CC_DESIGN_APPROVAL ( #5128, ( #6001 ) ) ;
#2912 = CARTESIAN_POINT ( 'NONE',  ( 2.969768487932331731E-17, 1.081250000000000044, 0.2425000000000000211 ) ) ;
#2913 = LOCAL_TIME ( 14, 45, 32.00000000000000000, #6452 ) ;
#2914 = TOROIDAL_SURFACE ( 'NONE', #3443, 0.2112499999999999933, 0.03125000000000000000 ) ;
#2915 = ORIENTED_EDGE ( 'NONE', *, *, #2287, .F. ) ;
#2916 = ORIENTED_EDGE ( 'NONE', *, *, #528, .F. ) ;
#2917 = ORIENTED_EDGE ( 'NONE', *, *, #5191, .F. ) ;
#2918 = CARTESIAN_POINT ( 'NONE',  ( 0.1250000000000000000, 1.530808498934191509E-17, 0.1250000000000000000 ) ) ;
#2919 = CARTESIAN_POINT ( 'NONE',  ( 0.000000000000000000, 1.112500000000000044, 0.000000000000000000 ) ) ;
#2920 = DATE_AND_TIME ( #2151, #318 ) ;
#2921 = DIRECTION ( 'NONE',  ( 0.000000000000000000, 0.000000000000000000, 1.000000000000000000 ) ) ;
#2922 = CIRCLE ( 'NONE', #3582, 0.2704878104020023710 ) ;
#2923 = ORIENTED_EDGE ( 'NONE', *, *, #578, .T. ) ;
#2924 = CIRCLE ( 'NONE', #7512, 0.03200000000000009781 ) ;
#2925 = ADVANCED_FACE ( 'NONE', ( #3404 ), #4667, .T. ) ;
#2926 = EDGE_CURVE ( 'NONE', #2089, #4761, #2242, .T. ) ;
#2927 = VECTOR ( 'NONE', #6631, 39.37007874015748143 ) ;
#2928 = CARTESIAN_POINT ( 'NONE',  ( 0.1000000000000000472, -0.03125000000000000000, 0.8125000000000000000 ) ) ;
#2929 = DIRECTION ( 'NONE',  ( -0.000000000000000000, -0.000000000000000000, 1.000000000000000000 ) ) ;
#2930 = DATE_AND_TIME ( #3929, #7996 ) ;
#2931 = DIRECTION ( 'NONE',  ( -1.000000000000000000, 0.000000000000000000, 0.000000000000000000 ) ) ;
#2932 = CARTESIAN_POINT ( 'NONE',  ( 1.437142212823555587, 1.212327995211809117, 0.2500000000000000000 ) ) ;
#2933 = ORIENTED_EDGE ( 'NONE', *, *, #5738, .F. ) ;
#2934 = PLANE ( 'NONE',  #550 ) ;
#2935 = CC_DESIGN_SECURITY_CLASSIFICATION ( #3335, ( #8099 ) ) ;
#2936 = EDGE_CURVE ( 'NONE', #6542, #2606, #1999, .T. ) ;
#2937 = AXIS2_PLACEMENT_3D ( 'NONE', #2928, #7318, #4778 ) ;
#2938 = FACE_OUTER_BOUND ( 'NONE', #653, .T. ) ;
#2939 = ADVANCED_FACE ( 'NONE', ( #6590 ), #7774, .T. ) ;
#2940 = ORIENTED_EDGE ( 'NONE', *, *, #899, .T. ) ;
#2941 = CLOSED_SHELL ( 'NONE', ( #3650, #7192, #226, #900, #7930, #6654, #4335, #4240, #827, #1873 ) ) ;
#2942 = VECTOR ( 'NONE', #5455, 39.37007874015748143 ) ;
#2943 = FACE_OUTER_BOUND ( 'NONE', #4650, .T. ) ;
#2944 = DIRECTION ( 'NONE',  ( -0.000000000000000000, -0.000000000000000000, 1.000000000000000000 ) ) ;
#2945 = DIRECTION ( 'NONE',  ( -0.000000000000000000, 0.000000000000000000, 1.000000000000000000 ) ) ;
#2946 = VERTEX_POINT ( 'NONE', #3964 ) ;
#2947 = ORIENTED_EDGE ( 'NONE', *, *, #4450, .F. ) ;
#2948 = CARTESIAN_POINT ( 'NONE',  ( -0.1250000000000000000, 0.6250000000000000000, 0.03125000000000000000 ) ) ;
#2949 = VECTOR ( 'NONE', #5800, 39.37007874015748143 ) ;
#2950 = AXIS2_PLACEMENT_3D ( 'NONE', #4216, #2985, #6715 ) ;
#2951 = CARTESIAN_POINT ( 'NONE',  ( 1.353816004522938599, 0.002313473902802895728, 0.000000000000000000 ) ) ;
#2952 = CARTESIAN_POINT ( 'NONE',  ( 1.537977733798261415, 1.853045334091375951, 0.0002768784213065589631 ) ) ;
#2953 = CIRCLE ( 'NONE', #7795, 0.1250000000000000000 ) ;
#2954 = PERSON_AND_ORGANIZATION ( #4735, #6190 ) ;
#2955 = ORIENTED_EDGE ( 'NONE', *, *, #1366, .F. ) ;
#2956 = DIRECTION ( 'NONE',  ( 0.000000000000000000, 0.000000000000000000, 1.000000000000000000 ) ) ;
#2957 = CARTESIAN_POINT ( 'NONE',  ( -0.04782642554762441683, -0.03125000000000000000, 0.07449999999999999678 ) ) ;
#2958 = CARTESIAN_POINT ( 'NONE',  ( 0.000000000000000000, 0.000000000000000000, 0.000000000000000000 ) ) ;
#2959 = EDGE_LOOP ( 'NONE', ( #6461, #7561, #1182, #7198 ) ) ;
#2960 = CIRCLE ( 'NONE', #3221, 0.3243589946935201418 ) ;
#2961 = CARTESIAN_POINT ( 'NONE',  ( 1.708525763102507256, 1.357565861344007141, 0.2042212951862970305 ) ) ;
#2962 = ORIENTED_EDGE ( 'NONE', *, *, #5383, .F. ) ;
#2963 = AXIS2_PLACEMENT_3D ( 'NONE', #2604, #5111, #6427 ) ;
#2964 = CIRCLE ( 'NONE', #88, 0.1799999999999999933 ) ;
#2965 = ORIENTED_EDGE ( 'NONE', *, *, #2679, .F. ) ;
#2966 = DIRECTION ( 'NONE',  ( 0.6568496200222107007, 0.7540216022612862279, -0.000000000000000000 ) ) ;
#2967 = CARTESIAN_POINT ( 'NONE',  ( 0.1024609768753887706, -0.4582992960660679516, 0.2195113138857777701 ) ) ;
#2968 = COORDINATED_UNIVERSAL_TIME_OFFSET ( 0, 0, .AHEAD. ) ;
#2969 = DIRECTION ( 'NONE',  ( -0.6930146854838814541, -0.5415747525370658844, -0.4758439167606253739 ) ) ;
#2970 = VERTEX_POINT ( 'NONE', #5979 ) ;
#2971 = AXIS2_PLACEMENT_3D ( 'NONE', #6174, #8039, #1859 ) ;
#2972 = PRODUCT ( 'Cleco, Fastener, Shell', 'Cleco, Fastener, Shell', '', ( #5396 ) ) ;
#2973 = CARTESIAN_POINT ( 'NONE',  ( 1.318949359038512847, 1.070937463555512004, -0.08001666686726011113 ) ) ;
#2974 = CARTESIAN_POINT ( 'NONE',  ( 0.1250000000000000000, 0.5625000000000000000, -0.03125000000000000000 ) ) ;
#2976 = CARTESIAN_POINT ( 'NONE',  ( 0.07000000000000002054, -0.03125000000000000000, 0.8125000000000000000 ) ) ;
#2975 = VECTOR ( 'NONE', #1491, 39.37007874015748854 ) ;
#2977 = PERSON_AND_ORGANIZATION_ROLE ( 'design_owner' ) ;
#2978 = CARTESIAN_POINT ( 'NONE',  ( 0.2386870781737283065, -0.03125000000000000000, 0.07449999999999999678 ) ) ;
#2979 = AXIS2_PLACEMENT_3D ( 'NONE', #136, #175, #2628 ) ;
#2980 = DIRECTION ( 'NONE',  ( 0.000000000000000000, 0.000000000000000000, 1.000000000000000000 ) ) ;
#2981 = EDGE_LOOP ( 'NONE', ( #2872, #4916, #7117, #3491 ) ) ;
#2982 = EDGE_CURVE ( 'NONE', #5415, #4005, #2266, .T. ) ;
#2983 = CARTESIAN_POINT ( 'NONE',  ( 1.534341089483872489, 1.136888306601122611, 0.1623010253712050266 ) ) ;
#2984 = DIRECTION ( 'NONE',  ( 0.7540216022612862279, -0.6568496200222105896, 0.000000000000000000 ) ) ;
#2985 = DIRECTION ( 'NONE',  ( 0.000000000000000000, 0.000000000000000000, 1.000000000000000000 ) ) ;
#2986 = EDGE_CURVE ( 'NONE', #141, #2877, #6850, .T. ) ;
#2987 = CARTESIAN_POINT ( 'NONE',  ( 1.264570944868384839, 1.043344531369262862, -0.06210292240206113229 ) ) ;
#2988 = DIRECTION ( 'NONE',  ( 1.000000000000000000, 0.000000000000000000, 0.000000000000000000 ) ) ;
#2989 = EDGE_CURVE ( 'NONE', #7979, #6859, #4368, .T. ) ;
#2990 = VERTEX_POINT ( 'NONE', #7242 ) ;
#2991 = EDGE_CURVE ( 'NONE', #2750, #845, #3433, .T. ) ;
#2992 = ORIENTED_EDGE ( 'NONE', *, *, #2586, .T. ) ;
#2993 = DIRECTION ( 'NONE',  ( -0.000000000000000000, -0.000000000000000000, -1.000000000000000000 ) ) ;
#2994 = APPROVAL ( #6052, 'UNSPECIFIED' ) ;
#2995 = EDGE_CURVE ( 'NONE', #3183, #6242, #2922, .T. ) ;
#2996 = CARTESIAN_POINT ( 'NONE',  ( -0.1249999999999999445, 0.03125000000000000000, 0.000000000000000000 ) ) ;
#2997 = DIRECTION ( 'NONE',  ( 0.7540216022612864499, -0.6568496200222104786, 0.000000000000000000 ) ) ;
#2998 = DATE_AND_TIME ( #2254, #5520 ) ;
#2999 = ORIENTED_EDGE ( 'NONE', *, *, #6434, .F. ) ;
#3000 = DIRECTION ( 'NONE',  ( 0.000000000000000000, 0.000000000000000000, -1.000000000000000000 ) ) ;
#3001 = LINE ( 'NONE', #6162, #3482 ) ;
#3002 = ORIENTED_EDGE ( 'NONE', *, *, #4851, .F. ) ;
#3003 = DIRECTION ( 'NONE',  ( -0.6568496200222107007, -0.7540216022612862279, 0.000000000000000000 ) ) ;
#3004 = ORIENTED_EDGE ( 'NONE', *, *, #4989, .F. ) ;
#3005 = B_SPLINE_CURVE_WITH_KNOTS ( 'NONE', 3,
 ( #4758, #2869, #995, #7256, #1636, #4223, #450, #5412, #4146, #6644 ),
 .UNSPECIFIED., .F., .F.,
 ( 4, 2, 2, 2, 4 ),
 ( 0.000000000000000000, 0.0003233994580137520723, 0.0006467989160275039277, 0.0009701983740412558916, 0.001293597832055007639 ),
 .UNSPECIFIED. ) ;
#3006 = CARTESIAN_POINT ( 'NONE',  ( -0.9280291358773672394, 0.8548654847802351631, -0.1250000000000000000 ) ) ;
#3007 = LENGTH_MEASURE_WITH_UNIT ( LENGTH_MEASURE( 0.02539999999999999897 ), #1120 );
#3008 = ORIENTED_EDGE ( 'NONE', *, *, #6903, .T. ) ;
#3009 = CARTESIAN_POINT ( 'NONE',  ( 0.6645694204159616758, 0.008319420416198241783, 0.07449999999999999678 ) ) ;
#3010 = PERSON_AND_ORGANIZATION_ROLE ( 'classification_officer' ) ;
#3011 = CARTESIAN_POINT ( 'NONE',  ( -1.040997396242602013, -0.7528336330030671597, 0.2222280897328365867 ) ) ;
#3012 = DIRECTION ( 'NONE',  ( -1.000000000000000000, 0.000000000000000000, 0.000000000000000000 ) ) ;
#3013 = CARTESIAN_POINT ( 'NONE',  ( -1.763177565995708296, 1.070083551578370207, -0.08100000000000007194 ) ) ;
#3014 = UNCERTAINTY_MEASURE_WITH_UNIT (LENGTH_MEASURE( 1.000000000000000082E-05 ), #1648, 'distance_accuracy_value', 'NONE');
#3015 = DIRECTION ( 'NONE',  ( -0.6568496200222103676, 0.7540216022612867830, 0.000000000000000000 ) ) ;
#3016 = APPROVAL_DATE_TIME ( #5607, #4591 ) ;
#3017 = FACE_OUTER_BOUND ( 'NONE', #1888, .T. ) ;
#3018 = CARTESIAN_POINT ( 'NONE',  ( -0.6495791112554195612, -0.6379566159512914947, 0.2179999999999999993 ) ) ;
#3019 = VERTEX_POINT ( 'NONE', #2862 ) ;
#3020 = CARTESIAN_POINT ( 'NONE',  ( 1.570659431541528983, 1.272357891351626913, 0.2374606253409364820 ) ) ;
#3021 = DIRECTION ( 'NONE',  ( -0.6568496200222107007, -0.7540216022612863389, 0.000000000000000000 ) ) ;
#3022 = DIRECTION ( 'NONE',  ( 0.000000000000000000, 0.000000000000000000, -1.000000000000000000 ) ) ;
#3023 = CARTESIAN_POINT ( 'NONE',  ( 1.316905486937928416, 1.070699082457407636, -0.07765199519505219805 ) ) ;
#3024 = DIRECTION ( 'NONE',  ( 0.6568496200222107007, 0.7540216022612863389, -0.000000000000000000 ) ) ;
#3025 = ORIENTED_EDGE ( 'NONE', *, *, #6995, .T. ) ;
#3026 = LINE ( 'NONE', #2948, #2389 ) ;
#3027 = EDGE_CURVE ( 'NONE', #4512, #1200, #6470, .T. ) ;
#3028 = EDGE_CURVE ( 'NONE', #1555, #6342, #5327, .T. ) ;
#3029 = DIRECTION ( 'NONE',  ( -0.6568496200222107007, -0.7540216022612862279, 0.000000000000000000 ) ) ;
#3030 = DIRECTION ( 'NONE',  ( -1.000000000000000000, 0.000000000000000000, 0.000000000000000000 ) ) ;
#3031 = COORDINATED_UNIVERSAL_TIME_OFFSET ( 0, 0, .AHEAD. ) ;
#3032 = VERTEX_POINT ( 'NONE', #5245 ) ;
#3033 = DIRECTION ( 'NONE',  ( 1.000000000000000000, -9.460047923712866088E-16, 0.000000000000000000 ) ) ;
#3034 = CARTESIAN_POINT ( 'NONE',  ( 0.2796912674003787513, -4.528516545235624413, 0.2500000000000000000 ) ) ;
#3035 = ORIENTED_EDGE ( 'NONE', *, *, #7687, .F. ) ;
#3036 = LINE ( 'NONE', #7984, #8009 ) ;
#3037 = CC_DESIGN_DATE_AND_TIME_ASSIGNMENT ( #8033, #7957, ( #1105 ) ) ;
#3038 = EDGE_CURVE ( 'NONE', #1048, #7187, #4705, .T. ) ;
#3039 = CC_DESIGN_APPROVAL ( #6755, ( #5523 ) ) ;
#3040 = EDGE_CURVE ( 'NONE', #4391, #3897, #7730, .T. ) ;
#3041 = VERTEX_POINT ( 'NONE', #3473 ) ;
#3042 = LINE ( 'NONE', #6130, #6982 ) ;
#3043 = APPROVAL_PERSON_ORGANIZATION ( #6072, #7704, #403 ) ;
#3044 = LOCAL_TIME ( 14, 45, 32.00000000000000000, #1945 ) ;
#3045 = CONTEXT_DEPENDENT_SHAPE_REPRESENTATION ( #3213, #7163 ) ;
#3046 = CARTESIAN_POINT ( 'NONE',  ( 0.000000000000000000, 0.000000000000000000, 0.1100000000000000006 ) ) ;
#3047 = ORIENTED_EDGE ( 'NONE', *, *, #8090, .F. ) ;
#3048 = AXIS2_PLACEMENT_3D ( 'NONE', #42, #3203, #2541 ) ;
#3049 = ORIENTED_EDGE ( 'NONE', *, *, #3534, .T. ) ;
#3050 = LINE ( 'NONE', #3712, #7524 ) ;
#3051 = DIRECTION ( 'NONE',  ( 0.000000000000000000, -0.000000000000000000, -1.000000000000000000 ) ) ;
#3052 = VECTOR ( 'NONE', #2993, 39.37007874015748143 ) ;
#3053 = DIRECTION ( 'NONE',  ( 0.000000000000000000, 0.000000000000000000, 1.000000000000000000 ) ) ;
#3054 = APPROVAL_DATE_TIME ( #6749, #7495 ) ;
#3055 = FACE_OUTER_BOUND ( 'NONE', #6272, .T. ) ;
#3056 = CARTESIAN_POINT ( 'NONE',  ( 1.587288320519282703, 1.780102713094158018, -0.02630007929079021534 ) ) ;
#3057 = ORIENTED_EDGE ( 'NONE', *, *, #7397, .F. ) ;
#3058 = DIRECTION ( 'NONE',  ( -1.000000000000000000, 0.000000000000000000, 0.000000000000000000 ) ) ;
#3059 = VECTOR ( 'NONE', #1240, 39.37007874015748854 ) ;
#3060 = ORIENTED_EDGE ( 'NONE', *, *, #1924, .F. ) ;
#3061 = CARTESIAN_POINT ( 'NONE',  ( 0.000000000000000000, 0.000000000000000000, 0.1250000000000000000 ) ) ;
#3062 = CARTESIAN_POINT ( 'NONE',  ( 1.244866787913109674, 1.068558539354471204, -0.06210292240210990578 ) ) ;
#3063 = VECTOR ( 'NONE', #7107, 39.37007874015748143 ) ;
#3064 = TOROIDAL_SURFACE ( 'NONE', #1353, 0.2468203157102362433, 0.03200000000000000067 ) ;
#3065 = DIRECTION ( 'NONE',  ( 1.000000000000000000, -0.000000000000000000, -0.000000000000000000 ) ) ;
#3066 = EDGE_LOOP ( 'NONE', ( #6690, #6809, #2153, #2461 ) ) ;
#3067 = DIRECTION ( 'NONE',  ( -0.000000000000000000, -0.000000000000000000, -1.000000000000000000 ) ) ;
#3068 = ADVANCED_FACE ( 'NONE', ( #3358 ), #2118, .F. ) ;
#3069 = ORGANIZATION ( 'NAUO-ORG7', 'UNSPECIFIED', 'UNSPECIFIED' ) ;
#3070 = AXIS2_PLACEMENT_3D ( 'NONE', #7666, #164, #950 ) ;
#3071 = CARTESIAN_POINT ( 'NONE',  ( 1.733157827467803669, 1.373632878365994348, 0.1887011865793609411 ) ) ;
#3072 = LINE ( 'NONE', #3732, #4815 ) ;
#3073 = PERSON_AND_ORGANIZATION ( #4735, #6190 ) ;
#3074 = ORIENTED_EDGE ( 'NONE', *, *, #1887, .F. ) ;
#3075 = CARTESIAN_POINT ( 'NONE',  ( 1.283086085828156087, 1.692381576688154032, -0.1039999999999998703 ) ) ;
#3076 = CARTESIAN_POINT ( 'NONE',  ( 1.780616048947831098, 1.055727875058976251, -0.08212881570848259982 ) ) ;
#3077 = CIRCLE ( 'NONE', #5960, 0.09374999999999998612 ) ;
#3078 = AXIS2_PLACEMENT_3D ( 'NONE', #2823, #1024, #6062 ) ;
#3079 = EDGE_LOOP ( 'NONE', ( #7013, #7033, #5944, #1564 ) ) ;
#3080 = CARTESIAN_POINT ( 'NONE',  ( -0.06999999999999996503, -0.03125000000000000000, 0.8125000000000000000 ) ) ;
#3081 = EDGE_CURVE ( 'NONE', #3933, #3711, #5899, .T. ) ;
#3082 = ADVANCED_FACE ( 'NONE', ( #2938 ), #2145, .T. ) ;
#3083 = ADVANCED_FACE ( 'NONE', ( #4297 ), #3322, .T. ) ;
#3084 = CARTESIAN_POINT ( 'NONE',  ( 1.806645078677039162, 1.428345690121396894, 0.1127449327592511957 ) ) ;
#3085 = CC_DESIGN_PERSON_AND_ORGANIZATION_ASSIGNMENT ( #8, #3821, ( #795 ) ) ;
#3086 =( NAMED_UNIT ( * ) SI_UNIT ( $, .STERADIAN. ) SOLID_ANGLE_UNIT ( ) );
#3087 = DIRECTION ( 'NONE',  ( 0.000000000000000000, 0.000000000000000000, -1.000000000000000000 ) ) ;
#3088 = EDGE_CURVE ( 'NONE', #3124, #2455, #3520, .T. ) ;
#3089 = APPROVAL_STATUS ( 'not_yet_approved' ) ;
#3090 = CARTESIAN_POINT ( 'NONE',  ( -1.723766588794375387, 1.115324847714046497, 0.1339999999999995361 ) ) ;
#3091 = AXIS2_PLACEMENT_3D ( 'NONE', #3034, #6680, #7426 ) ;
#3092 = ADVANCED_FACE ( 'NONE', ( #6107 ), #1172, .F. ) ;
#3093 = EDGE_CURVE ( 'NONE', #3518, #2827, #3644, .T. ) ;
#3094 = VECTOR ( 'NONE', #5208, 39.37007874015748143 ) ;
#3095 = ORIENTED_EDGE ( 'NONE', *, *, #4943, .F. ) ;
#3096 = ORIENTED_EDGE ( 'NONE', *, *, #4249, .F. ) ;
#3097 = CARTESIAN_POINT ( 'NONE',  ( 0.000000000000000000, -0.03125000000000000000, 0.3061494484901324808 ) ) ;
#3098 = AXIS2_PLACEMENT_3D ( 'NONE', #5707, #3932, #84 ) ;
#3099 = DIRECTION ( 'NONE',  ( -0.6568496200222107007, -0.7540216022612862279, 0.000000000000000000 ) ) ;
#3100 = UNCERTAINTY_MEASURE_WITH_UNIT (LENGTH_MEASURE( 1.000000000000000082E-05 ), #7434, 'distance_accuracy_value', 'NONE');
#3101 = DIRECTION ( 'NONE',  ( -1.000000000000000000, 0.000000000000000000, 0.000000000000000000 ) ) ;
#3102 = APPROVAL_ROLE ( '' ) ;
#3103 = FACE_OUTER_BOUND ( 'NONE', #4682, .T. ) ;
#3104 = CARTESIAN_POINT ( 'NONE',  ( 1.589183446880458206, 1.785275342778416929, -0.05425644835043919034 ) ) ;
#3105 = ORIENTED_EDGE ( 'NONE', *, *, #1316, .F. ) ;
#3106 = CIRCLE ( 'NONE', #4286, 0.03125000000000000694 ) ;
#3107 = AXIS2_PLACEMENT_3D ( 'NONE', #6356, #2607, #3274 ) ;
#3108 = DIRECTION ( 'NONE',  ( -1.000000000000000000, 0.000000000000000000, 0.000000000000000000 ) ) ;
#3109 = AXIS2_PLACEMENT_3D ( 'NONE', #2557, #5799, #1362 ) ;
#3110 = AXIS2_PLACEMENT_3D ( 'NONE', #639, #1088, #545 ) ;
#3111 = ORIENTED_EDGE ( 'NONE', *, *, #4127, .F. ) ;
#3112 = CARTESIAN_POINT ( 'NONE',  ( 0.1250000000000000000, 0.5625000000000000000, -0.03125000000000000000 ) ) ;
#3113 = CARTESIAN_POINT ( 'NONE',  ( 1.323123159461853326, 1.089031584755306259, -0.1264980700302772432 ) ) ;
#3114 = CARTESIAN_POINT ( 'NONE',  ( -2.022862211726251136, 1.296302217412564017, 0.1339999999999995917 ) ) ;
#3115 = ORIENTED_EDGE ( 'NONE', *, *, #1078, .F. ) ;
#3116 = EDGE_LOOP ( 'NONE', ( #7035, #6079, #3328, #885 ) ) ;
#3117 = TOROIDAL_SURFACE ( 'NONE', #7034, 0.09374999999999998612, 0.03125000000000000000 ) ;
#3118 = CARTESIAN_POINT ( 'NONE',  ( 6.067840808230170246, 0.2405569712445295161, 0.1850000000000003586 ) ) ;
#3119 = ORIENTED_EDGE ( 'NONE', *, *, #1880, .T. ) ;
#3120 = DIMENSIONAL_EXPONENTS ( 1.000000000000000000, 0.000000000000000000, 0.000000000000000000, 0.000000000000000000, 0.000000000000000000, 0.000000000000000000, 0.000000000000000000 ) ;
#3121 = CARTESIAN_POINT ( 'NONE',  ( 4.013019369095008670, -4.147396371033809537, 0.1250000000000000000 ) ) ;
#3122 = CARTESIAN_POINT ( 'NONE',  ( 0.000000000000000000, 0.000000000000000000, 0.000000000000000000 ) ) ;
#3123 = COORDINATED_UNIVERSAL_TIME_OFFSET ( 0, 0, .AHEAD. ) ;
#3124 = VERTEX_POINT ( 'NONE', #436 ) ;
#3125 = CARTESIAN_POINT ( 'NONE',  ( 0.2386870781737283065, -0.03125000000000000000, 0.07449999999999999678 ) ) ;
#3126 = LINE ( 'NONE', #1427, #4797 ) ;
#3127 = ORIENTED_EDGE ( 'NONE', *, *, #1481, .T. ) ;
#3128 = PLANE ( 'NONE',  #2645 ) ;
#3129 = ORIENTED_EDGE ( 'NONE', *, *, #4090, .T. ) ;
#3130 = CARTESIAN_POINT ( 'NONE',  ( 1.822942581281881136, 1.440962976019389608, 0.08718017679867827441 ) ) ;
#3131 = DIRECTION ( 'NONE',  ( -1.000000000000000000, -0.000000000000000000, -0.000000000000000000 ) ) ;
#3132 = COORDINATED_UNIVERSAL_TIME_OFFSET ( 0, 0, .AHEAD. ) ;
#3133 = DIRECTION ( 'NONE',  ( -0.7879377495398141029, -0.6157549048526802515, 0.000000000000000000 ) ) ;
#3134 = EDGE_LOOP ( 'NONE', ( #7282, #2860, #1371, #2553 ) ) ;
#3135 = ORIENTED_EDGE ( 'NONE', *, *, #1538, .F. ) ;
#3136 = CARTESIAN_POINT ( 'NONE',  ( 1.339249842318065653, 1.071711091725345621, -0.1040000000000607383 ) ) ;
#3137 = CARTESIAN_POINT ( 'NONE',  ( 0.000000000000000000, 0.000000000000000000, -0.6537499999999999423 ) ) ;
#3138 = EDGE_CURVE ( 'NONE', #789, #6271, #7885, .T. ) ;
#3139 = ADVANCED_FACE ( 'NONE', ( #2894 ), #5400, .F. ) ;
#3140 = DIRECTION ( 'NONE',  ( 0.000000000000000000, 0.000000000000000000, 1.000000000000000000 ) ) ;
#3141 = APPROVAL_STATUS ( 'not_yet_approved' ) ;
#3142 = DIRECTION ( 'NONE',  ( -0.4606913525677331367, -0.8875604078987033851, 0.000000000000000000 ) ) ;
#3143 = CARTESIAN_POINT ( 'NONE',  ( 1.820728631330852609, 1.486631279361974478, -0.03246653637537286891 ) ) ;
#3144 = ADVANCED_FACE ( 'NONE', ( #6668 ), #6144, .T. ) ;
#3145 = EDGE_LOOP ( 'NONE', ( #8004, #3874, #505, #971, #4106, #3253, #8087, #7722 ) ) ;
#3146 = APPROVAL ( #4435, 'UNSPECIFIED' ) ;
#3147 = ORIENTED_EDGE ( 'NONE', *, *, #7481, .F. ) ;
#3148 = EDGE_CURVE ( 'NONE', #6628, #5472, #4173, .T. ) ;
#3149 = ORIENTED_EDGE ( 'NONE', *, *, #3936, .F. ) ;
#3150 = CARTESIAN_POINT ( 'NONE',  ( -1.723766588794375387, 1.115324847714046497, -0.08100000000000007194 ) ) ;
#3151 = FACE_OUTER_BOUND ( 'NONE', #2398, .T. ) ;
#3152 = CARTESIAN_POINT ( 'NONE',  ( 2.204364238465235822E-17, 0.000000000000000000, 0.1799999999999999933 ) ) ;
#3153 = ORIENTED_EDGE ( 'NONE', *, *, #598, .F. ) ;
#3154 = PLANE ( 'NONE',  #700 ) ;
#3155 = DIRECTION ( 'NONE',  ( 0.000000000000000000, 0.000000000000000000, -1.000000000000000000 ) ) ;
#3156 = CARTESIAN_POINT ( 'NONE',  ( -1.983451234524918450, 1.341543513548241418, 0.1339999999999995917 ) ) ;
#3157 = SHAPE_DEFINITION_REPRESENTATION ( #3552, #1942 ) ;
#3158 = ORIENTED_EDGE ( 'NONE', *, *, #123, .T. ) ;
#3159 = CARTESIAN_POINT ( 'NONE',  ( 1.360211532822002800, 1.082033417235804373, -0.1575618645360782888 ) ) ;
#3160 = CYLINDRICAL_SURFACE ( 'NONE', #4411, 0.1150000000000000050 ) ;
#3161 = EDGE_LOOP ( 'NONE', ( #1327, #2940, #7959, #1591, #6867, #7613, #5130, #3559 ) ) ;
#3162 = DIRECTION ( 'NONE',  ( 0.7540216022612862279, -0.6568496200222105896, 0.000000000000000000 ) ) ;
#3163 = LOCAL_TIME ( 14, 45, 32.00000000000000000, #6011 ) ;
#3164 = ORIENTED_EDGE ( 'NONE', *, *, #6600, .T. ) ;
#3165 = FACE_OUTER_BOUND ( 'NONE', #6805, .T. ) ;
#3166 = CARTESIAN_POINT ( 'NONE',  ( 1.780616048947831986, 1.055727875058976917, -0.1039999999999998703 ) ) ;
#3167 = APPROVAL_DATE_TIME ( #3210, #4489 ) ;
#3168 = CARTESIAN_POINT ( 'NONE',  ( 1.554085806680376436, 0.9967294227056006095, -0.1039999999999998287 ) ) ;
#3169 = AXIS2_PLACEMENT_3D ( 'NONE', #4265, #3652, #6149 ) ;
#3170 = ORIENTED_EDGE ( 'NONE', *, *, #3936, .T. ) ;
#3171 = ORIENTED_EDGE ( 'NONE', *, *, #1235, .T. ) ;
#3172 = DIRECTION ( 'NONE',  ( -0.000000000000000000, -0.000000000000000000, -1.000000000000000000 ) ) ;
#3173 =( LENGTH_UNIT ( ) NAMED_UNIT ( * ) SI_UNIT ( $, .METRE. ) );
#3174 = CARTESIAN_POINT ( 'NONE',  ( 1.408343819019455843E-17, 0.6350000000000000089, 0.1150000000000000050 ) ) ;
#3175 = PERSON_AND_ORGANIZATION ( #4735, #6190 ) ;
#3176 = DIRECTION ( 'NONE',  ( 0.000000000000000000, 0.000000000000000000, 1.000000000000000000 ) ) ;
#3177 = CARTESIAN_POINT ( 'NONE',  ( 1.800320205903116921, 1.030513867073702183, -0.08212881570848259982 ) ) ;
#3178 = VECTOR ( 'NONE', #1309, 39.37007874015748143 ) ;
#3179 = EDGE_CURVE ( 'NONE', #5222, #5561, #5420, .T. ) ;
#3180 = EDGE_CURVE ( 'NONE', #4881, #761, #5678, .T. ) ;
#3181 = CIRCLE ( 'NONE', #1482, 0.06199999999999999956 ) ;
#3182 = DIRECTION ( 'NONE',  ( 0.000000000000000000, 0.000000000000000000, 1.000000000000000000 ) ) ;
#3183 = VERTEX_POINT ( 'NONE', #1021 ) ;
#3184 = CARTESIAN_POINT ( 'NONE',  ( -0.1875000000000000278, 2.296212748401287726E-17, -0.6849999999999999423 ) ) ;
#3185 = CC_DESIGN_PERSON_AND_ORGANIZATION_ASSIGNMENT ( #5672, #6404, ( #187 ) ) ;
#3186 = LINE ( 'NONE', #649, #2440 ) ;
#3187 = EDGE_CURVE ( 'NONE', #7167, #2507, #5519, .T. ) ;
#3188 = EDGE_CURVE ( 'NONE', #5187, #6273, #7409, .T. ) ;
#3189 = CARTESIAN_POINT ( 'NONE',  ( -0.6148017326439689789, 0.2092266780087954636, 0.03199999999999999373 ) ) ;
#3190 = ORIENTED_EDGE ( 'NONE', *, *, #6642, .T. ) ;
#3191 = VECTOR ( 'NONE', #6778, 39.37007874015748854 ) ;
#3192 = PLANE ( 'NONE',  #5016 ) ;
#3193 = CIRCLE ( 'NONE', #8025, 0.3243589946935201418 ) ;
#3194 = CIRCLE ( 'NONE', #7773, 0.1487499999999999933 ) ;
#3195 = ORIENTED_EDGE ( 'NONE', *, *, #5339, .F. ) ;
#3196 = CARTESIAN_POINT ( 'NONE',  ( 0.7510138408322231118, -0.03124999999962550443, 0.07449999999999999678 ) ) ;
#3197 = DIRECTION ( 'NONE',  ( -0.6157549048526801405, 0.7879377495398142139, 0.000000000000000000 ) ) ;
#3198 = APPROVAL_STATUS ( 'not_yet_approved' ) ;
#3199 = ORIENTED_EDGE ( 'NONE', *, *, #4127, .T. ) ;
#3200 = DIRECTION ( 'NONE',  ( -1.000000000000000000, 1.224646799147352961E-16, 0.000000000000000000 ) ) ;
#3201 = ADVANCED_FACE ( 'NONE', ( #395, #2278 ), #4791, .T. ) ;
#3202 = CARTESIAN_POINT ( 'NONE',  ( 2.587066363198783776E-17, 1.081250000000000044, 0.2112499999999999933 ) ) ;
#3203 = DIRECTION ( 'NONE',  ( 0.6157549048526804736, -0.7879377495398138809, -0.000000000000000000 ) ) ;
#3204 = APPROVAL_PERSON_ORGANIZATION ( #5966, #6203, #1573 ) ;
#3205 = AXIS2_PLACEMENT_3D ( 'NONE', #7768, #7166, #1548 ) ;
#3206 = DIRECTION ( 'NONE',  ( -1.000000000000000000, 0.000000000000000000, 0.000000000000000000 ) ) ;
#3207 = DIRECTION ( 'NONE',  ( -0.6568496200222100345, -0.7540216022612867830, -1.579971258330007776E-15 ) ) ;
#3208 = LINE ( 'NONE', #1312, #7896 ) ;
#3209 = AXIS2_PLACEMENT_3D ( 'NONE', #1958, #2452, #3813 ) ;
#3210 = DATE_AND_TIME ( #7510, #2279 ) ;
#3211 = CARTESIAN_POINT ( 'NONE',  ( 0.000000000000000000, 1.081250000000000044, 0.000000000000000000 ) ) ;
#3212 = ORIENTED_EDGE ( 'NONE', *, *, #1546, .F. ) ;
#3213 =( REPRESENTATION_RELATIONSHIP ('NONE','NONE', #3360, #2774 ) REPRESENTATION_RELATIONSHIP_WITH_TRANSFORMATION ( #4820 )SHAPE_REPRESENTATION_RELATIONSHIP( ) );
#3214 = AXIS2_PLACEMENT_3D ( 'NONE', #6132, #1077, #1241 ) ;
#3215 = AXIS2_PLACEMENT_3D ( 'NONE', #6419, #6343, #800 ) ;
#3216 = EDGE_LOOP ( 'NONE', ( #4430, #1698, #3455 ) ) ;
#3217 = DIRECTION ( 'NONE',  ( -0.9584282785752022971, -0.2853335501257686646, 0.000000000000000000 ) ) ;
#3218 = PERSON_AND_ORGANIZATION ( #4735, #6190 ) ;
#3219 = PLANE ( 'NONE',  #3109 ) ;
#3220 = CARTESIAN_POINT ( 'NONE',  ( 1.472947776714219836, 0.7825821671288679671, 0.1850000000000003586 ) ) ;
#3221 = AXIS2_PLACEMENT_3D ( 'NONE', #3866, #169, #7557 ) ;
#3222 = VERTEX_POINT ( 'NONE', #2716 ) ;
#3223 = CIRCLE ( 'NONE', #5058, 0.1799999999999999933 ) ;
#3224 = VERTEX_POINT ( 'NONE', #1650 ) ;
#3225 = CARTESIAN_POINT ( 'NONE',  ( 1.780616048947831986, 1.055727875058976917, -0.1039999999999998703 ) ) ;
#3226 = ORIENTED_EDGE ( 'NONE', *, *, #6942, .T. ) ;
#3228 = CARTESIAN_POINT ( 'NONE',  ( 1.718386282410942600, 1.375744605918879593, 0.2061739259319994577 ) ) ;
#3227 = VECTOR ( 'NONE', #4217, 39.37007874015748143 ) ;
#3229 = LINE ( 'NONE', #147, #5854 ) ;
#3230 = AXIS2_PLACEMENT_3D ( 'NONE', #3713, #4289, #2349 ) ;
#3231 = EDGE_CURVE ( 'NONE', #4366, #1756, #3847, .T. ) ;
#3232 = ADVANCED_FACE ( 'NONE', ( #7223 ), #6722, .T. ) ;
#3233 = CARTESIAN_POINT ( 'NONE',  ( 2.387087291339119677, -6.013863021948615106, 0.1250000000000000000 ) ) ;
#3234 = AXIS2_PLACEMENT_3D ( 'NONE', #977, #4056, #6556 ) ;
#3235 = CARTESIAN_POINT ( 'NONE',  ( 1.773383007244042631, 1.432796503982046943, 0.1500871045907652412 ) ) ;
#3236 = DIRECTION ( 'NONE',  ( -0.7540216022612862279, 0.6568496200222109227, 0.000000000000000000 ) ) ;
#3237 = APPROVAL_DATE_TIME ( #2537, #4952 ) ;
#3238 = ADVANCED_FACE ( 'NONE', ( #2147 ), #306, .T. ) ;
#3239 = VERTEX_POINT ( 'NONE', #3999 ) ;
#3240 = ADVANCED_FACE ( 'NONE', ( #4076 ), #4601, .F. ) ;
#3241 = DIRECTION ( 'NONE',  ( 1.224646799147353207E-16, 1.000000000000000000, -0.000000000000000000 ) ) ;
#3242 = CARTESIAN_POINT ( 'NONE',  ( -1.196132095472828727, -0.2317400473908176328, 0.2500000000000001110 ) ) ;
#3243 = ORIENTED_EDGE ( 'NONE', *, *, #3394, .T. ) ;
#3244 = FACE_OUTER_BOUND ( 'NONE', #7407, .T. ) ;
#3245 = CC_DESIGN_PERSON_AND_ORGANIZATION_ASSIGNMENT ( #7403, #4291, ( #1211 ) ) ;
#3246 = ADVANCED_FACE ( 'NONE', ( #2754 ), #5387, .T. ) ;
#3247 = DIRECTION ( 'NONE',  ( 0.000000000000000000, 0.000000000000000000, 1.000000000000000000 ) ) ;
#3248 = DIRECTION ( 'NONE',  ( 8.538331638034394400E-19, -4.597438515588352722E-19, -1.000000000000000000 ) ) ;
#3249 = FACE_OUTER_BOUND ( 'NONE', #151, .T. ) ;
#3250 = CARTESIAN_POINT ( 'NONE',  ( -2.114821033088378321, 1.190739337094255168, 0.1339999999999995917 ) ) ;
#3251 = CARTESIAN_POINT ( 'NONE',  ( 1.713744337812789009, 1.365763491892051373, 0.1712939242540917617 ) ) ;
#3252 = EDGE_LOOP ( 'NONE', ( #2386, #1616, #7507, #7068 ) ) ;
#3253 = ORIENTED_EDGE ( 'NONE', *, *, #3285, .F. ) ;
#3254 = CARTESIAN_POINT ( 'NONE',  ( 0.000000000000000000, 0.000000000000000000, -0.1250000000000000000 ) ) ;
#3255 = CARTESIAN_POINT ( 'NONE',  ( -0.6148017326439689789, 0.2092266780087954636, 0.2179999999999999993 ) ) ;
#3256 = CALENDAR_DATE ( 2026, 9, 10 ) ;
#3257 = FACE_OUTER_BOUND ( 'NONE', #7113, .T. ) ;
#3258 = LINE ( 'NONE', #4455, #5825 ) ;
#3259 = ORIENTED_EDGE ( 'NONE', *, *, #6005, .F. ) ;
#3260 = EDGE_CURVE ( 'NONE', #774, #2343, #7631, .T. ) ;
#3261 = ORIENTED_EDGE ( 'NONE', *, *, #4536, .F. ) ;
#3262 = DIRECTION ( 'NONE',  ( -0.000000000000000000, 1.000000000000000000, -0.000000000000000000 ) ) ;
#3263 = VERTEX_POINT ( 'NONE', #3386 ) ;
#3264 = PLANE ( 'NONE',  #3723 ) ;
#3265 = CARTESIAN_POINT ( 'NONE',  ( 2.056298385200680201, 0.7198786976815831906, -0.09374999999999998612 ) ) ;
#3266 = DIRECTION ( 'NONE',  ( 0.4606913525677331367, 0.8875604078987033851, 0.000000000000000000 ) ) ;
#3267 = ORIENTED_EDGE ( 'NONE', *, *, #21, .F. ) ;
#3268 = CARTESIAN_POINT ( 'NONE',  ( -0.1255000000000000282, 0.000000000000000000, -0.6219999999999999973 ) ) ;
#3269 = ORIENTED_EDGE ( 'NONE', *, *, #5287, .T. ) ;
#3270 = CARTESIAN_POINT ( 'NONE',  ( 1.781945410564037768, 1.422047848568809059, 0.1506494843211809709 ) ) ;
#3271 = CARTESIAN_POINT ( 'NONE',  ( -0.03921911030312481838, -0.4592703903598064352, 0.2500000000000000000 ) ) ;
#3272 = APPROVAL_DATE_TIME ( #2741, #6755 ) ;
#3273 = VERTEX_POINT ( 'NONE', #5880 ) ;
#3274 = DIRECTION ( 'NONE',  ( 1.000000000000000000, 0.000000000000000000, 0.000000000000000000 ) ) ;
#3275 = DIRECTION ( 'NONE',  ( 0.000000000000000000, 0.000000000000000000, -1.000000000000000000 ) ) ;
#3276 = ORIENTED_EDGE ( 'NONE', *, *, #7078, .F. ) ;
#3277 = CARTESIAN_POINT ( 'NONE',  ( 1.493295815665055759, 1.213146689595488326, 0.2319700209806794811 ) ) ;
#3278 = EDGE_CURVE ( 'NONE', #3971, #5356, #7758, .T. ) ;
#3279 = EDGE_CURVE ( 'NONE', #7259, #141, #4628, .T. ) ;
#3280 = DIRECTION ( 'NONE',  ( -0.000000000000000000, -1.000000000000000000, -0.000000000000000000 ) ) ;
#3281 = CALENDAR_DATE ( 2026, 9, 10 ) ;
#3282 = CARTESIAN_POINT ( 'NONE',  ( 0.1054677083281892608, 0.000000000000000000, 0.03125000000000000000 ) ) ;
#3283 = CC_DESIGN_DATE_AND_TIME_ASSIGNMENT ( #383, #3459, ( #2562 ) ) ;
#3284 = DIRECTION ( 'NONE',  ( -1.000000000000000000, 0.000000000000000000, 0.000000000000000000 ) ) ;
#3285 = EDGE_CURVE ( 'NONE', #4233, #1238, #7154, .T. ) ;
#3286 = PRODUCT ( 'Cleco, Fastener, Pincher', 'Cleco, Fastener, Pincher', '', ( #2796 ) ) ;
#3287 = DIRECTION ( 'NONE',  ( 1.000000000000000000, 0.000000000000000000, 0.000000000000000000 ) ) ;
#3288 = ADVANCED_FACE ( 'NONE', ( #3420 ), #7891, .T. ) ;
#3289 = B_SPLINE_CURVE_WITH_KNOTS ( 'NONE', 3,
 ( #4693, #4079, #302, #4657, #4003, #3507 ),
 .UNSPECIFIED., .F., .F.,
 ( 4, 2, 4 ),
 ( 1.256969020782943308E-21, 0.0003533183248413553470, 0.0007066366496827106939 ),
 .UNSPECIFIED. ) ;
#3290 = ORIENTED_EDGE ( 'NONE', *, *, #5448, .F. ) ;
#3291 = CARTESIAN_POINT ( 'NONE',  ( 0.000000000000000000, 0.000000000000000000, 0.000000000000000000 ) ) ;
#3292 = ORIENTED_EDGE ( 'NONE', *, *, #4342, .F. ) ;
#3293 = CARTESIAN_POINT ( 'NONE',  ( 1.684866161243239846, 1.178252195112418299, -0.1039999999999998703 ) ) ;
#3294 = APPLICATION_PROTOCOL_DEFINITION ( 'international standard', 'config_control_design', 1994, #1541 ) ;
#3295 = CYLINDRICAL_SURFACE ( 'NONE', #7296, 0.03199999999999986189 ) ;
#3296 = CARTESIAN_POINT ( 'NONE',  ( -1.040997396242601791, -0.7528336330030669377, 0.2500000000000000000 ) ) ;
#3297 = ORIENTED_EDGE ( 'NONE', *, *, #7785, .F. ) ;
#3298 = VERTEX_POINT ( 'NONE', #5964 ) ;
#3299 = ORIENTED_EDGE ( 'NONE', *, *, #691, .T. ) ;
#3300 =( GEOMETRIC_REPRESENTATION_CONTEXT ( 3 ) GLOBAL_UNCERTAINTY_ASSIGNED_CONTEXT ( ( #3100 ) ) GLOBAL_UNIT_ASSIGNED_CONTEXT ( ( #7434, #5504, #6734 ) ) REPRESENTATION_CONTEXT ( 'NONE', 'WORKASPACE' ) );
#3301 = CC_DESIGN_SECURITY_CLASSIFICATION ( #5523, ( #5925 ) ) ;
#3302 = ORIENTED_EDGE ( 'NONE', *, *, #7300, .F. ) ;
#3303 = CARTESIAN_POINT ( 'NONE',  ( 0.000000000000000000, 0.03124999999999997571, -0.1150000000000000050 ) ) ;
#3304 = ORIENTED_EDGE ( 'NONE', *, *, #4050, .T. ) ;
#3305 = CIRCLE ( 'NONE', #954, 0.03199999999999997985 ) ;
#3306 = CARTESIAN_POINT ( 'NONE',  ( 1.612360986893233372, 1.332289325118119150, 0.2442303131640376490 ) ) ;
#3307 = CARTESIAN_POINT ( 'NONE',  ( 1.358097358395378151, 1.070245242547174680, -0.1269261509454146786 ) ) ;
#3308 = CARTESIAN_POINT ( 'NONE',  ( 3.221700243049673507, 0.8684880333666036289, -0.1849999999999999978 ) ) ;
#3309 = DIRECTION ( 'NONE',  ( 1.000000000000000000, -0.000000000000000000, 1.224646799147353207E-16 ) ) ;
#3310 = AXIS2_PLACEMENT_3D ( 'NONE', #8046, #3333, #5832 ) ;
#3311 = ORIENTED_EDGE ( 'NONE', *, *, #3279, .F. ) ;
#3312 = CARTESIAN_POINT ( 'NONE',  ( 1.518800558058658989, 1.876586918424175465, -0.003115248787935155639 ) ) ;
#3313 = DIRECTION ( 'NONE',  ( -0.7879377495398138809, -0.6157549048526803626, 0.000000000000000000 ) ) ;
#3314 = PERSON_AND_ORGANIZATION_ROLE ( 'classification_officer' ) ;
#3315 = ORIENTED_EDGE ( 'NONE', *, *, #2432, .F. ) ;
#3316 = VECTOR ( 'NONE', #1804, 39.37007874015748143 ) ;
#3317 = CARTESIAN_POINT ( 'NONE',  ( 1.411244833761398310, 1.056435878372752324, -0.1949596646313069837 ) ) ;
#3318 = CARTESIAN_POINT ( 'NONE',  ( -0.1250000000000000000, 0.000000000000000000, 0.1250000000000000000 ) ) ;
#3319 = VERTEX_POINT ( 'NONE', #5357 ) ;
#3320 = ORIENTED_EDGE ( 'NONE', *, *, #4798, .T. ) ;
#3321 = DIRECTION ( 'NONE',  ( 0.000000000000000000, -0.000000000000000000, 1.000000000000000000 ) ) ;
#3322 = TOROIDAL_SURFACE ( 'NONE', #7374, 0.2923589946935198913, 0.03200000000000000067 ) ;
#3323 = ORIENTED_EDGE ( 'NONE', *, *, #576, .T. ) ;
#3324 = ORIENTED_EDGE ( 'NONE', *, *, #5442, .T. ) ;
#3325 = LINE ( 'NONE', #6296, #852 ) ;
#3326 = CARTESIAN_POINT ( 'NONE',  ( 0.000000000000000000, 0.000000000000000000, -0.5599999999999999423 ) ) ;
#3327 = CALENDAR_DATE ( 2026, 9, 10 ) ;
#3328 = ORIENTED_EDGE ( 'NONE', *, *, #21, .T. ) ;
#3329 = ADVANCED_FACE ( 'NONE', ( #299 ), #5315, .T. ) ;
#3330 = DIRECTION ( 'NONE',  ( -0.000000000000000000, -0.000000000000000000, -1.000000000000000000 ) ) ;
#3331 = AXIS2_PLACEMENT_3D ( 'NONE', #6501, #7632, #2555 ) ;
#3332 = VECTOR ( 'NONE', #2237, 39.37007874015747433 ) ;
#3333 = DIRECTION ( 'NONE',  ( 1.224646799147353207E-16, 1.000000000000000000, -0.000000000000000000 ) ) ;
#3334 = ORIENTED_EDGE ( 'NONE', *, *, #4243, .T. ) ;
#3335 = SECURITY_CLASSIFICATION ( '', '', #6211 ) ;
#3336 = AXIS2_PLACEMENT_3D ( 'NONE', #8038, #1245, #7400 ) ;
#3337 = ORIENTED_EDGE ( 'NONE', *, *, #7796, .T. ) ;
#3338 = EDGE_CURVE ( 'NONE', #6611, #3346, #5565, .T. ) ;
#3339 = SHAPE_REPRESENTATION_RELATIONSHIP ( 'NONE' , 'NONE' ,  #2298, #2787 ) ;
#3340 = DIRECTION ( 'NONE',  ( 1.000000000000000000, 0.000000000000000000, 0.000000000000000000 ) ) ;
#3341 = PERSON_AND_ORGANIZATION_ROLE ( 'classification_officer' ) ;
#3342 = LINE ( 'NONE', #4809, #6126 ) ;
#3343 = DIRECTION ( 'NONE',  ( -1.000000000000000000, 0.000000000000000000, 0.000000000000000000 ) ) ;
#3344 = EDGE_CURVE ( 'NONE', #7381, #4612, #1043, .T. ) ;
#3345 = ORIENTED_EDGE ( 'NONE', *, *, #6198, .T. ) ;
#3346 = VERTEX_POINT ( 'NONE', #6853 ) ;
#3347 = CIRCLE ( 'NONE', #2819, 0.3024878104020024550 ) ;
#3348 = ORIENTED_EDGE ( 'NONE', *, *, #6423, .F. ) ;
#3349 = EDGE_CURVE ( 'NONE', #1006, #445, #1160, .T. ) ;
#3350 = EDGE_LOOP ( 'NONE', ( #1156, #1364, #5284, #4503, #7870, #7939, #7105, #388, #5889 ) ) ;
#3351 = ORIENTED_EDGE ( 'NONE', *, *, #69, .T. ) ;
#3352 = FACE_OUTER_BOUND ( 'NONE', #7820, .T. ) ;
#3353 = AXIS2_PLACEMENT_3D ( 'NONE', #508, #2969, #7471 ) ;
#3354 = ORIENTED_EDGE ( 'NONE', *, *, #2801, .F. ) ;
#3355 = CARTESIAN_POINT ( 'NONE',  ( 1.717034119172104800, 1.391647134812390663, 0.2009755516559021404 ) ) ;
#3356 = CARTESIAN_POINT ( 'NONE',  ( -1.763177565995707630, 1.070083551578369763, -0.08100000000000007194 ) ) ;
#3357 = FACE_OUTER_BOUND ( 'NONE', #5537, .T. ) ;
#3358 = FACE_OUTER_BOUND ( 'NONE', #6812, .T. ) ;
#3359 = CIRCLE ( 'NONE', #4271, 0.3099999999999745737 ) ;
#3360 = SHAPE_REPRESENTATION ( 'MAS-157', ( #3706, #2642, #7098, #5791, #161, #3437, #1460, #3562 ), #8006 ) ;
#3361 = AXIS2_PLACEMENT_3D ( 'NONE', #1557, #2865, #7207 ) ;
#3362 = AXIS2_PLACEMENT_3D ( 'NONE', #2005, #2588, #2613 ) ;
#3363 = CARTESIAN_POINT ( 'NONE',  ( 1.406322310917426543, 1.749149093313088876, 0.2028435978050005528 ) ) ;
#3364 = DIRECTION ( 'NONE',  ( 8.881784197001252323E-16, 0.000000000000000000, 1.000000000000000000 ) ) ;
#3365 = CALENDAR_DATE ( 2026, 9, 10 ) ;
#3366 = ORIENTED_EDGE ( 'NONE', *, *, #7629, .T. ) ;
#3367 = DIRECTION ( 'NONE',  ( -0.000000000000000000, -1.000000000000000000, -0.000000000000000000 ) ) ;
#3368 = CARTESIAN_POINT ( 'NONE',  ( 0.3553155032461795537, -0.3420189219808928982, 0.02497744489995550390 ) ) ;
#3369 = ORIENTED_EDGE ( 'NONE', *, *, #4091, .F. ) ;
#3370 = VECTOR ( 'NONE', #548, 39.37007874015748143 ) ;
#3371 = DIRECTION ( 'NONE',  ( -1.000000000000000000, 0.000000000000000000, 0.000000000000000000 ) ) ;
#3372 = AXIS2_PLACEMENT_3D ( 'NONE', #3636, #1822, #1700 ) ;
#3373 = AXIS2_PLACEMENT_3D ( 'NONE', #7404, #4864, #4781 ) ;
#3374 = DIRECTION ( 'NONE',  ( 0.6157549048526801405, -0.7879377495398141029, -0.000000000000000000 ) ) ;
#3375 = AXIS2_PLACEMENT_3D ( 'NONE', #7376, #6195, #4843 ) ;
#3376 = CARTESIAN_POINT ( 'NONE',  ( -1.543211452806561690, 0.6927940070358462599, 0.1250000000000000000 ) ) ;
#3377 = PERSON_AND_ORGANIZATION ( #4735, #6190 ) ;
#3378 = VERTEX_POINT ( 'NONE', #5424 ) ;
#3379 = CARTESIAN_POINT ( 'NONE',  ( 0.3517571870377138588, -0.3450675717666435438, 0.2305015624669528862 ) ) ;
#3380 = CARTESIAN_POINT ( 'NONE',  ( 1.537181070339166844, 1.279018903020961329, 0.2500000000000000000 ) ) ;
#3381 = EDGE_CURVE ( 'NONE', #4761, #3273, #2418, .T. ) ;
#3382 = ADVANCED_FACE ( 'NONE', ( #1851 ), #5942, .T. ) ;
#3383 = EDGE_LOOP ( 'NONE', ( #5345, #4476, #6514, #5444 ) ) ;
#3384 = ORIENTED_EDGE ( 'NONE', *, *, #6979, .F. ) ;
#3385 = EDGE_CURVE ( 'NONE', #658, #3319, #7435, .T. ) ;
#3386 = CARTESIAN_POINT ( 'NONE',  ( 1.384649234319611288, 1.035652040038434807, -0.08212881570848259982 ) ) ;
#3387 = CARTESIAN_POINT ( 'NONE',  ( 1.400692579910243429, 1.149720402410526976, 0.2179999999999999716 ) ) ;
#3388 = PERSON_AND_ORGANIZATION_ROLE ( 'classification_officer' ) ;
#3389 = DIRECTION ( 'NONE',  ( 0.000000000000000000, 0.000000000000000000, -1.000000000000000000 ) ) ;
#3390 = CYLINDRICAL_SURFACE ( 'NONE', #3868, 0.1799999999999999933 ) ;
#3391 = ADVANCED_FACE ( 'NONE', ( #8031 ), #3666, .T. ) ;
#3392 = ORIENTED_EDGE ( 'NONE', *, *, #3601, .F. ) ;
#3393 = ORIENTED_EDGE ( 'NONE', *, *, #6152, .T. ) ;
#3394 = EDGE_CURVE ( 'NONE', #3711, #3298, #3042, .T. ) ;
#3395 = EDGE_CURVE ( 'NONE', #1110, #1116, #1694, .T. ) ;
#3396 = ORIENTED_EDGE ( 'NONE', *, *, #994, .F. ) ;
#3397 = DIRECTION ( 'NONE',  ( 0.9726399823210830631, 0.2323175946639496336, 0.000000000000000000 ) ) ;
#3398 = EDGE_CURVE ( 'NONE', #5902, #661, #1816, .T. ) ;
#3399 = CARTESIAN_POINT ( 'NONE',  ( 1.655550958614606438, 1.357113354811811057, 0.2318296825077736378 ) ) ;
#3400 = CARTESIAN_POINT ( 'NONE',  ( 2.778417425565558062E-17, 1.050000000000000044, 0.2112499999999999933 ) ) ;
#3401 = PRODUCT_RELATED_PRODUCT_CATEGORY ( 'detail', '', ( #6511 ) ) ;
#3402 = DIRECTION ( 'NONE',  ( 0.9987955914953423608, 0.04906492035527378059, 0.000000000000000000 ) ) ;
#3403 = EDGE_CURVE ( 'NONE', #4974, #1559, #4499, .T. ) ;
#3404 = FACE_OUTER_BOUND ( 'NONE', #4793, .T. ) ;
#3405 = CARTESIAN_POINT ( 'NONE',  ( 1.290439921825005554, 1.657739327948754671, 0.2499999999999999722 ) ) ;
#3406 = DIRECTION ( 'NONE',  ( 0.7879377495398141029, 0.6157549048526801405, 0.000000000000000000 ) ) ;
#3407 = COORDINATED_UNIVERSAL_TIME_OFFSET ( 0, 0, .AHEAD. ) ;
#3408 = CYLINDRICAL_SURFACE ( 'NONE', #3752, 0.3750000000001075251 ) ;
#3409 = CARTESIAN_POINT ( 'NONE',  ( -0.1250000000000000000, 0.6250000000000000000, 0.000000000000000000 ) ) ;
#3410 = EDGE_LOOP ( 'NONE', ( #4869, #5613, #7522, #5572, #1317, #3057 ) ) ;
#3411 = CARTESIAN_POINT ( 'NONE',  ( 0.000000000000000000, 0.000000000000000000, -0.5599999999999999423 ) ) ;
#3412 = CARTESIAN_POINT ( 'NONE',  ( -1.601062921509531556, 0.9288608832735947285, -0.08100000000000007194 ) ) ;
#3413 = CARTESIAN_POINT ( 'NONE',  ( 1.492515782973882432, 1.856045982048359688, -0.05383208248477879682 ) ) ;
#3414 = APPROVAL_ROLE ( '' ) ;
#3415 = VERTEX_POINT ( 'NONE', #2918 ) ;
#3416 = CARTESIAN_POINT ( 'NONE',  ( 0.3566525292043902229, -0.3408511508279103985, 0.2216499829201352689 ) ) ;
#3417 = CARTESIAN_POINT ( 'NONE',  ( 1.463490907143538688, 1.192314464452256972, 0.2277028927441933914 ) ) ;
#3418 = ORIENTED_EDGE ( 'NONE', *, *, #2329, .T. ) ;
#3419 = VERTEX_POINT ( 'NONE', #2306 ) ;
#3420 = FACE_OUTER_BOUND ( 'NONE', #3608, .T. ) ;
#3421 = CARTESIAN_POINT ( 'NONE',  ( 1.400692579910243651, 1.149720402410526754, 0.2500000000000000000 ) ) ;
#3422 = COORDINATED_UNIVERSAL_TIME_OFFSET ( 0, 0, .AHEAD. ) ;
#3423 = DIRECTION ( 'NONE',  ( -1.000000000000000000, -1.762482576557733776E-15, 0.000000000000000000 ) ) ;
#3424 = ORIENTED_EDGE ( 'NONE', *, *, #3788, .F. ) ;
#3425 = VERTEX_POINT ( 'NONE', #3705 ) ;
#3426 = EDGE_LOOP ( 'NONE', ( #3512, #1436 ) ) ;
#3427 = DIRECTION ( 'NONE',  ( -1.000000000000000000, 0.000000000000000000, 0.000000000000000000 ) ) ;
#3428 = VERTEX_POINT ( 'NONE', #6209 ) ;
#3429 = DIRECTION ( 'NONE',  ( -0.000000000000000000, 1.000000000000000000, -0.000000000000000000 ) ) ;
#3430 = DIRECTION ( 'NONE',  ( 0.6568496200222108117, 0.7540216022612861169, 0.000000000000000000 ) ) ;
#3431 = CYLINDRICAL_SURFACE ( 'NONE', #7485, 0.03124999999999999306 ) ;
#3432 = ADVANCED_FACE ( 'NONE', ( #7469 ), #4360, .F. ) ;
#3433 = LINE ( 'NONE', #190, #6460 ) ;
#3434 = LOCAL_TIME ( 14, 45, 32.00000000000000000, #1227 ) ;
#3435 = AXIS2_PLACEMENT_3D ( 'NONE', #4577, #2861, #6523 ) ;
#3436 = APPROVAL ( #5712, 'UNSPECIFIED' ) ;
#3437 = AXIS2_PLACEMENT_3D ( 'NONE', #2614, #3207, #6290 ) ;
#3438 = CARTESIAN_POINT ( 'NONE',  ( 1.466665248995881354, 0.6909135088951505743, 0.1250000000000000000 ) ) ;
#3439 = LOCAL_TIME ( 14, 45, 32.00000000000000000, #4904 ) ;
#3440 = DIRECTION ( 'NONE',  ( -1.000000000000000000, 0.000000000000000000, 0.000000000000000000 ) ) ;
#3441 = DIRECTION ( 'NONE',  ( 0.000000000000000000, 0.000000000000000000, -1.000000000000000000 ) ) ;
#3442 = ORIENTED_EDGE ( 'NONE', *, *, #4050, .F. ) ;
#3443 = AXIS2_PLACEMENT_3D ( 'NONE', #6034, #1688, #5381 ) ;
#3444 = CARTESIAN_POINT ( 'NONE',  ( 1.411244833761398310, 1.056435878372752324, -0.1949596646313069837 ) ) ;
#3445 = CIRCLE ( 'NONE', #7371, 0.3099400561648077423 ) ;
#3446 = CARTESIAN_POINT ( 'NONE',  ( -0.5068880400889234084, 2.974486634375206329, 0.000000000000000000 ) ) ;
#3447 = CYLINDRICAL_SURFACE ( 'NONE', #1666, 8.513908398499120622 ) ;
#3448 = PERSON_AND_ORGANIZATION_ROLE ( 'design_owner' ) ;
#3449 = ORIENTED_EDGE ( 'NONE', *, *, #2669, .T. ) ;
#3450 = CARTESIAN_POINT ( 'NONE',  ( 0.3265987596359649636, -0.3651148059186102857, 0.2456569822661065772 ) ) ;
#3451 = CARTESIAN_POINT ( 'NONE',  ( 1.571814533976791495, 1.273076930690883124, 0.2372021369713644967 ) ) ;
#3452 = ORIENTED_EDGE ( 'NONE', *, *, #3990, .F. ) ;
#3453 = VECTOR ( 'NONE', #2209, 39.37007874015748143 ) ;
#3454 = ORIENTED_EDGE ( 'NONE', *, *, #7151, .T. ) ;
#3455 = ORIENTED_EDGE ( 'NONE', *, *, #6328, .F. ) ;
#3456 = ORIENTED_EDGE ( 'NONE', *, *, #3532, .T. ) ;
#3457 = CARTESIAN_POINT ( 'NONE',  ( -4.882388066182494768, 5.670153330992220297, 0.3125000000000000000 ) ) ;
#3458 = CARTESIAN_POINT ( 'NONE',  ( 1.652539028737726179, 1.219618926967090289, -0.1039999999999998703 ) ) ;
#3459 = DATE_TIME_ROLE ( 'classification_date' ) ;
#3460 = CARTESIAN_POINT ( 'NONE',  ( 0.000000000000000000, 0.000000000000000000, 0.000000000000000000 ) ) ;
#3461 = ORIENTED_EDGE ( 'NONE', *, *, #4180, .T. ) ;
#3462 = VERTEX_POINT ( 'NONE', #8073 ) ;
#3463 = CC_DESIGN_SECURITY_CLASSIFICATION ( #1357, ( #8096 ) ) ;
#3464 = VECTOR ( 'NONE', #5258, 39.37007874015748854 ) ;
#3465 = ORIENTED_EDGE ( 'NONE', *, *, #7536, .T. ) ;
#3466 = FACE_OUTER_BOUND ( 'NONE', #7816, .T. ) ;
#3467 = DIRECTION ( 'NONE',  ( -0.2873478855663426645, -0.000000000000000000, 0.9578262852211522071 ) ) ;
#3468 = CARTESIAN_POINT ( 'NONE',  ( -1.411841654243101596, 0.8435981834898315102, 0.1250000000000000000 ) ) ;
#3469 = VECTOR ( 'NONE', #1425, 39.37007874015748143 ) ;
#3470 = VECTOR ( 'NONE', #1303, 39.37007874015748143 ) ;
#3471 = EDGE_LOOP ( 'NONE', ( #6464, #5044, #1809, #59 ) ) ;
#3472 = CARTESIAN_POINT ( 'NONE',  ( 6.190221022838899856, 0.4584861219976859026, 5.393636709996481038 ) ) ;
#3473 = CARTESIAN_POINT ( 'NONE',  ( 2.036190745269639724, 1.255453516974595507, -0.08212881570848257207 ) ) ;
#3474 = APPLICATION_CONTEXT ( 'configuration controlled 3d designs of mechanical parts and assemblies' ) ;
#3475 = CIRCLE ( 'NONE', #6485, 0.3243589946935200308 ) ;
#3476 = VERTEX_POINT ( 'NONE', #1074 ) ;
#3477 = ADVANCED_FACE ( 'NONE', ( #5468 ), #7955, .T. ) ;
#3478 = CARTESIAN_POINT ( 'NONE',  ( 1.530808498934191201E-17, 1.362500000000000044, -0.1250000000000000000 ) ) ;
#3479 = DIRECTION ( 'NONE',  ( 1.000000000000000000, 1.092739197465705090E-15, 0.000000000000000000 ) ) ;
#3480 = EDGE_CURVE ( 'NONE', #5415, #1006, #1618, .T. ) ;
#3481 = DIRECTION ( 'NONE',  ( -1.000000000000000000, 0.000000000000000000, -0.000000000000000000 ) ) ;
#3482 = VECTOR ( 'NONE', #4229, 39.37007874015748143 ) ;
#3483 = ORIENTED_EDGE ( 'NONE', *, *, #5248, .F. ) ;
#3484 = LINE ( 'NONE', #400, #1089 ) ;
#3485 = AXIS2_PLACEMENT_3D ( 'NONE', #7328, #4956, #441 ) ;
#3486 = EDGE_CURVE ( 'NONE', #4578, #3378, #3194, .T. ) ;
#3487 = VECTOR ( 'NONE', #5334, 39.37007874015748143 ) ;
#3488 = EDGE_CURVE ( 'NONE', #6170, #4537, #6084, .T. ) ;
#3489 = CARTESIAN_POINT ( 'NONE',  ( 0.1250000000000000278, 0.03125000000000000000, 0.06250000000000000000 ) ) ;
#3490 = CALENDAR_DATE ( 2026, 9, 10 ) ;
#3491 = ORIENTED_EDGE ( 'NONE', *, *, #3846, .F. ) ;
#3492 = EDGE_CURVE ( 'NONE', #4775, #2827, #7515, .T. ) ;
#3493 = AXIS2_PLACEMENT_3D ( 'NONE', #1092, #8042, #2931 ) ;
#3494 = VECTOR ( 'NONE', #663, 39.37007874015748143 ) ;
#3495 = CARTESIAN_POINT ( 'NONE',  ( 0.3495743270459968910, -0.3469141170041438738, 0.2327060356060121626 ) ) ;
#3496 = PRODUCT_DEFINITION_SHAPE ( 'NONE', 'NONE',  #7247 ) ;
#3497 = CARTESIAN_POINT ( 'NONE',  ( -0.6570132742846659379, -0.6068321365170169512, 0.2500000000000000000 ) ) ;
#3498 = PRODUCT_DEFINITION ( 'UNKNOWN', '', #4611, #7276 ) ;
#3499 = ADVANCED_FACE ( 'NONE', ( #1774 ), #6362, .F. ) ;
#3500 = CIRCLE ( 'NONE', #752, 0.1250000000000000000 ) ;
#3501 = VERTEX_POINT ( 'NONE', #784 ) ;
#3502 =( NAMED_UNIT ( * ) SI_UNIT ( $, .STERADIAN. ) SOLID_ANGLE_UNIT ( ) );
#3503 = EDGE_LOOP ( 'NONE', ( #5892, #4854, #5145, #2140 ) ) ;
#3504 = DIRECTION ( 'NONE',  ( -1.000000000000000000, 1.224646799147352714E-16, 0.000000000000000000 ) ) ;
#3505 = LINE ( 'NONE', #5426, #7560 ) ;
#3506 = APPROVAL_STATUS ( 'not_yet_approved' ) ;
#3507 = CARTESIAN_POINT ( 'NONE',  ( 1.859753234433174418, 1.471617347716406288, -0.009971652696953780398 ) ) ;
#3508 = ORIENTED_EDGE ( 'NONE', *, *, #6491, .F. ) ;
#3509 = AXIS2_PLACEMENT_3D ( 'NONE', #3697, #7543, #3033 ) ;
#3510 = ORIENTED_EDGE ( 'NONE', *, *, #2432, .T. ) ;
#3511 = CIRCLE ( 'NONE', #1023, 0.03200000000000009781 ) ;
#3512 = ORIENTED_EDGE ( 'NONE', *, *, #69, .F. ) ;
#3513 = CARTESIAN_POINT ( 'NONE',  ( -0.1249999999999999445, -0.03125000000000000000, 0.000000000000000000 ) ) ;
#3514 = DESIGN_CONTEXT ( 'detailed design', #7559, 'design' ) ;
#3515 = CARTESIAN_POINT ( 'NONE',  ( 0.000000000000000000, 0.6124999999999999334, 0.1250000000000000000 ) ) ;
#3516 = DIRECTION ( 'NONE',  ( 0.7540216022612867830, -0.6568496200222101455, -1.912293595564982478E-15 ) ) ;
#3517 = ORIENTED_EDGE ( 'NONE', *, *, #7785, .T. ) ;
#3518 = VERTEX_POINT ( 'NONE', #7669 ) ;
#3519 = DIRECTION ( 'NONE',  ( -0.6568496200222107007, -0.7540216022612862279, 0.000000000000000000 ) ) ;
#3520 = LINE ( 'NONE', #5481, #1882 ) ;
#3521 = DIRECTION ( 'NONE',  ( -0.000000000000000000, -0.000000000000000000, 1.000000000000000000 ) ) ;
#3522 = DIRECTION ( 'NONE',  ( -0.000000000000000000, -0.000000000000000000, -1.000000000000000000 ) ) ;
#3523 = FACE_OUTER_BOUND ( 'NONE', #3216, .T. ) ;
#3524 = EDGE_LOOP ( 'NONE', ( #5628, #568 ) ) ;
#3525 = LINE ( 'NONE', #7179, #6846 ) ;
#3526 = FACE_BOUND ( 'NONE', #5617, .T. ) ;
#3527 = LINE ( 'NONE', #4185, #7431 ) ;
#3528 = COORDINATED_UNIVERSAL_TIME_OFFSET ( 0, 0, .AHEAD. ) ;
#3529 = EDGE_LOOP ( 'NONE', ( #5835, #2598, #5885, #3889 ) ) ;
#3530 = CARTESIAN_POINT ( 'NONE',  ( 0.000000000000000000, 0.6124999999999999334, -0.03125000000000000000 ) ) ;
#3531 = DIRECTION ( 'NONE',  ( 0.000000000000000000, 0.000000000000000000, 1.000000000000000000 ) ) ;
#3532 = EDGE_CURVE ( 'NONE', #646, #255, #6603, .T. ) ;
#3533 = EDGE_CURVE ( 'NONE', #3419, #6385, #1720, .T. ) ;
#3534 = EDGE_CURVE ( 'NONE', #3946, #7900, #5813, .T. ) ;
#3535 = ORIENTED_EDGE ( 'NONE', *, *, #7397, .T. ) ;
#3536 = EDGE_CURVE ( 'NONE', #1501, #4570, #167, .T. ) ;
#3537 = ORIENTED_EDGE ( 'NONE', *, *, #1127, .T. ) ;
#3538 = CARTESIAN_POINT ( 'NONE',  ( 0.000000000000000000, 0.6124999999999999334, 0.000000000000000000 ) ) ;
#3539 = DIRECTION ( 'NONE',  ( 0.000000000000000000, 0.000000000000000000, 1.000000000000000000 ) ) ;
#3540 = COORDINATED_UNIVERSAL_TIME_OFFSET ( 0, 0, .AHEAD. ) ;
#3541 = DIRECTION ( 'NONE',  ( -0.000000000000000000, -1.000000000000000000, -0.000000000000000000 ) ) ;
#3542 = CARTESIAN_POINT ( 'NONE',  ( 1.400692579912386826, 1.149720402407784059, 0.2179999999999999438 ) ) ;
#3543 = DIRECTION ( 'NONE',  ( -0.000000000000000000, -1.000000000000000000, -0.000000000000000000 ) ) ;
#3544 = APPLICATION_PROTOCOL_DEFINITION ( 'international standard', 'config_control_design', 1994, #6566 ) ;
#3545 = FACE_OUTER_BOUND ( 'NONE', #2681, .T. ) ;
#3546 = CARTESIAN_POINT ( 'NONE',  ( -0.1250000000000000000, 0.5625000000000000000, -0.03125000000000000000 ) ) ;
#3547 = ORIENTED_EDGE ( 'NONE', *, *, #3983, .T. ) ;
#3548 = CARTESIAN_POINT ( 'NONE',  ( 1.543023339786947723, 1.143323475675890322, 0.1681221971056049980 ) ) ;
#3549 = DIRECTION ( 'NONE',  ( 0.000000000000000000, -1.000000000000000000, 0.000000000000000000 ) ) ;
#3550 = SECURITY_CLASSIFICATION ( '', '', #6159 ) ;
#3551 = ORIENTED_EDGE ( 'NONE', *, *, #6513, .F. ) ;
#3552 = PRODUCT_DEFINITION_SHAPE ( 'NONE', 'NONE',  #830 ) ;
#3553 = DIRECTION ( 'NONE',  ( 0.9726399823210830631, 0.2323175946639496336, 0.000000000000000000 ) ) ;
#3554 = CARTESIAN_POINT ( 'NONE',  ( 1.321405161348359947, 1.071700536256935843, -0.1133567676827914872 ) ) ;
#3555 = AXIS2_PLACEMENT_3D ( 'NONE', #5720, #6981, #135 ) ;
#3556 = LOCAL_TIME ( 14, 45, 32.00000000000000000, #3031 ) ;
#3557 = CARTESIAN_POINT ( 'NONE',  ( -1.463573652696772642, 0.6234192589057615530, -0.1918577977169502180 ) ) ;
#3558 = ORIENTED_EDGE ( 'NONE', *, *, #669, .T. ) ;
#3559 = ORIENTED_EDGE ( 'NONE', *, *, #7200, .T. ) ;
#3560 = DIRECTION ( 'NONE',  ( -0.7879377495398142139, -0.6157549048526801405, 0.000000000000000000 ) ) ;
#3561 = CIRCLE ( 'NONE', #292, 0.5000000000000279776 ) ;
#3562 = AXIS2_PLACEMENT_3D ( 'NONE', #2589, #664, #1900 ) ;
#3563 = CARTESIAN_POINT ( 'NONE',  ( 0.000000000000000000, -0.03125000000000000000, 0.2896281645421511231 ) ) ;
#3564 = CARTESIAN_POINT ( 'NONE',  ( 1.535032449692323997, 1.849374163788637837, -0.03177454249412108023 ) ) ;
#3565 = APPLICATION_PROTOCOL_DEFINITION ( 'international standard', 'config_control_design', 1994, #702 ) ;
#3566 = ORIENTED_EDGE ( 'NONE', *, *, #6494, .F. ) ;
#3567 = AXIS2_PLACEMENT_3D ( 'NONE', #6892, #2656, #1430 ) ;
#3568 = DIRECTION ( 'NONE',  ( 0.000000000000000000, -1.000000000000000000, 0.000000000000000000 ) ) ;
#3569 = CYLINDRICAL_SURFACE ( 'NONE', #4922, 0.1204106507132265275 ) ;
#3570 = CARTESIAN_POINT ( 'NONE',  ( 1.569959517566582363, 0.8504923821133684170, -0.08212881570848257207 ) ) ;
#3571 = LOCAL_TIME ( 14, 45, 32.00000000000000000, #1909 ) ;
#3572 = B_SPLINE_CURVE_WITH_KNOTS ( 'NONE', 3,
 ( #5625, #3242, #3902, #2654, #3781, #1890, #5160, #5046 ),
 .UNSPECIFIED., .F., .F.,
 ( 4, 2, 2, 4 ),
 ( 2.742838647325547832E-18, 0.0003234044359150124292, 0.0006468088718300220395, 0.001293617743660035839 ),
 .UNSPECIFIED. ) ;
#3573 = AXIS2_PLACEMENT_3D ( 'NONE', #3689, #4221, #7894 ) ;
#3574 = VERTEX_POINT ( 'NONE', #7587 ) ;
#3575 = MANIFOLD_SOLID_BREP ( 'Fillet2', #326 ) ;
#3576 = ADVANCED_FACE ( 'NONE', ( #3249 ), #6900, .F. ) ;
#3577 = ORIENTED_EDGE ( 'NONE', *, *, #2015, .T. ) ;
#3578 = CARTESIAN_POINT ( 'NONE',  ( -1.332203854133312548, 0.7742234353597469143, -0.1918577977169502180 ) ) ;
#3579 = CARTESIAN_POINT ( 'NONE',  ( 0.1009400014640523119, -0.4585254034878745721, 0.2212619352215731139 ) ) ;
#3580 = APPROVAL_ROLE ( '' ) ;
#3581 = FACE_OUTER_BOUND ( 'NONE', #3410, .T. ) ;
#3582 = AXIS2_PLACEMENT_3D ( 'NONE', #315, #6471, #2821 ) ;
#3583 = CC_DESIGN_PERSON_AND_ORGANIZATION_ASSIGNMENT ( #7978, #2906, ( #172 ) ) ;
#3584 = AXIS2_PLACEMENT_3D ( 'NONE', #5433, #3543, #430 ) ;
#3585 = ORIENTED_EDGE ( 'NONE', *, *, #6491, .T. ) ;
#3586 = AXIS2_PLACEMENT_3D ( 'NONE', #6341, #798, #7724 ) ;
#3587 = FACE_OUTER_BOUND ( 'NONE', #1522, .T. ) ;
#3588 = DIRECTION ( 'NONE',  ( 0.000000000000000000, 0.000000000000000000, -1.000000000000000000 ) ) ;
#3589 = EDGE_CURVE ( 'NONE', #7415, #6720, #6347, .T. ) ;
#3590 = DIRECTION ( 'NONE',  ( 1.000000000000000000, 0.000000000000000000, 0.000000000000000000 ) ) ;
#3591 = DATE_TIME_ROLE ( 'creation_date' ) ;
#3593 = MANIFOLD_SOLID_BREP ( 'Boss-Extrude1', #2941 ) ;
#3592 = LINE ( 'NONE', #6099, #3370 ) ;
#3594 = ORIENTED_EDGE ( 'NONE', *, *, #4388, .T. ) ;
#3595 = VERTEX_POINT ( 'NONE', #5750 ) ;
#3596 = DIRECTION ( 'NONE',  ( -1.000000000000000000, 0.000000000000000000, 0.000000000000000000 ) ) ;
#3597 = ORGANIZATION ( 'NAUO-ORG6', 'UNSPECIFIED', 'UNSPECIFIED' ) ;
#3598 = AXIS2_PLACEMENT_3D ( 'NONE', #5670, #4473, #2007 ) ;
#3599 = CARTESIAN_POINT ( 'NONE',  ( 1.780616048947831098, 1.055727875058976251, -0.08212881570848259982 ) ) ;
#3600 = PRODUCT_DEFINITION ( 'UNKNOWN', '', #1857, #308 ) ;
#3601 = EDGE_CURVE ( 'NONE', #5356, #4366, #4443, .T. ) ;
#3602 = AXIS2_PLACEMENT_3D ( 'NONE', #4487, #1445, #2106 ) ;
#3603 = VECTOR ( 'NONE', #5603, 39.37007874015748143 ) ;
#3604 = LINE ( 'NONE', #4750, #6614 ) ;
#3605 = LINE ( 'NONE', #5522, #4030 ) ;
#3606 = DIRECTION ( 'NONE',  ( -0.6568496200222107007, -0.7540216022612862279, 0.000000000000000000 ) ) ;
#3607 = ORIENTED_EDGE ( 'NONE', *, *, #5350, .F. ) ;
#3608 = EDGE_LOOP ( 'NONE', ( #3730, #4958, #3740, #5225 ) ) ;
#3609 = CARTESIAN_POINT ( 'NONE',  ( 1.630463830202529829, 1.227750391954798070, 0.1987711295701233005 ) ) ;
#3610 = AXIS2_PLACEMENT_3D ( 'NONE', #969, #5884, #4163 ) ;
#3611 = CIRCLE ( 'NONE', #327, 0.3750000000000000555 ) ;
#3612 = DIRECTION ( 'NONE',  ( 0.000000000000000000, 0.000000000000000000, 1.000000000000000000 ) ) ;
#3613 = CARTESIAN_POINT ( 'NONE',  ( 6.067840808230170246, 0.2405569712445295161, 5.393636709996481038 ) ) ;
#3614 = AXIS2_PLACEMENT_3D ( 'NONE', #97, #211, #7511 ) ;
#3615 = CALENDAR_DATE ( 2026, 9, 10 ) ;
#3616 = EDGE_LOOP ( 'NONE', ( #5007, #841, #6092, #1002, #3775, #1447, #1041, #1728 ) ) ;
#3617 = CARTESIAN_POINT ( 'NONE',  ( -0.1250000000000000000, 0.5625000000000000000, 0.03125000000000000000 ) ) ;
#3618 = LINE ( 'NONE', #2458, #3872 ) ;
#3619 = CARTESIAN_POINT ( 'NONE',  ( 1.570113095412482451, 1.303985922897850758, 0.2500000000000000555 ) ) ;
#3620 = CIRCLE ( 'NONE', #5189, 0.2500000000000000555 ) ;
#3621 =( BOUNDED_SURFACE ( )  B_SPLINE_SURFACE ( 3, 2, ( 
 ( #1170, #4908, #2983 ),
 ( #1623, #4172, #3548 ),
 ( #435, #5440, #7927 ),
 ( #2324, #4831, #2355 ),
 ( #7324, #1706, #3680 ),
 ( #516, #6709, #8005 ),
 ( #6753, #480, #4867 ),
 ( #3020, #6179, #1748 ),
 ( #4256, #552, #1139 ),
 ( #6142, #5518, #7408 ),
 ( #4296, #5368, #7624 ),
 ( #8088, #6493, #2012 ),
 ( #4950, #7673, #6407 ),
 ( #1210, #4982, #6364 ),
 ( #7449, #4519, #3719 ),
 ( #7020, #5175, #4373 ),
 ( #6226, #3251, #2062 ),
 ( #751, #2099, #4598 ) ),
 .UNSPECIFIED., .F., .F., .F. ) 
 B_SPLINE_SURFACE_WITH_KNOTS ( ( 4, 2, 2, 2, 2, 2, 2, 2, 4 ),
 ( 3, 3 ),
 ( 0.005269457407105175052, 0.006547192405793211822, 0.007824927404481247725, 0.009102662403169283628, 0.01038039740185731953, 0.01165813240054535543, 0.01293586739923339307, 0.01421360239792142897, 0.01549133739660946488 ),
 ( 0.1429062507207413957, 0.9470558914401250306 ),
 .UNSPECIFIED. ) 
 GEOMETRIC_REPRESENTATION_ITEM ( )  RATIONAL_B_SPLINE_SURFACE ( (
 ( 0.9282505022062121913, 0.7600379373203958178, 0.9706280646979809079),
 ( 0.9343171304435629043, 0.7803274260291386266, 0.9731115470576900961),
 ( 0.9397170595443995467, 0.7983871778769424665, 0.9753221042471091895),
 ( 0.9491101166107969167, 0.8298017162058096696, 0.9791673195158672183),
 ( 0.9531118816443266972, 0.8431853888632105942, 0.9808055133328683617),
 ( 0.9595828167972388911, 0.8648270587634172557, 0.9834545059321079252),
 ( 0.9620129929284466641, 0.8729546428587842133, 0.9844493418305206855),
 ( 0.9652734486511969081, 0.8838590492248784569, 0.9857840674730465880),
 ( 0.9661037643372263339, 0.8866359922115385483, 0.9861239719930808834),
 ( 0.9661130461342239961, 0.8866670346469766040, 0.9861277716620581169),
 ( 0.9652745230984527414, 0.8838626426518387813, 0.9857845073171743744),
 ( 0.9620007201733109525, 0.8729135973361294987, 0.9844443177595388894),
 ( 0.9595699749684953872, 0.8647841100068597298, 0.9834492489007055083),
 ( 0.9531660649921475104, 0.8433666019490960730, 0.9808276942516981345),
 ( 0.9491742944624668166, 0.8300163553341466383, 0.9791935918629224300),
 ( 0.9397117968768438079, 0.7983695771884257164, 0.9753199498803788448),
 ( 0.9342913856339358780, 0.7802413239962128211, 0.9731010079611670527),
 ( 0.9282505022067131240, 0.7600379373220710333, 0.9706280646981859661) ) ) 
 REPRESENTATION_ITEM ( '' )  SURFACE ( )  );
#3622 = VERTEX_POINT ( 'NONE', #6323 ) ;
#3623 = ORIENTED_EDGE ( 'NONE', *, *, #562, .F. ) ;
#3624 = AXIS2_PLACEMENT_3D ( 'NONE', #5864, #1589, #2124 ) ;
#3625 = VECTOR ( 'NONE', #1349, 39.37007874015748143 ) ;
#3626 = CARTESIAN_POINT ( 'NONE',  ( 15385.36825653051164, -19685.23544977528218, -0.3750000000000000555 ) ) ;
#3627 =( CONVERSION_BASED_UNIT ( 'INCH', #4970 ) LENGTH_UNIT ( ) NAMED_UNIT ( #6210 ) );
#3628 = ORIENTED_EDGE ( 'NONE', *, *, #3480, .F. ) ;
#3629 = DIRECTION ( 'NONE',  ( 0.000000000000000000, -1.000000000000000000, 0.000000000000000000 ) ) ;
#3630 = APPROVAL_DATE_TIME ( #4936, #5699 ) ;
#3631 = CARTESIAN_POINT ( 'NONE',  ( -1.040997396242601791, -0.7528336330030669377, 0.2179999999999999993 ) ) ;
#3632 = VECTOR ( 'NONE', #7238, 39.37007874015748143 ) ;
#3633 = ORIENTED_EDGE ( 'NONE', *, *, #4788, .F. ) ;
#3634 = ORIENTED_EDGE ( 'NONE', *, *, #482, .F. ) ;
#3635 = CARTESIAN_POINT ( 'NONE',  ( 6.067385397437120353, 0.2407432673787524013, -0.1250000000000000000 ) ) ;
#3636 = CARTESIAN_POINT ( 'NONE',  ( 0.6645694204159616758, 0.008319420416198241783, 0.07449999999999999678 ) ) ;
#3638 = DIRECTION ( 'NONE',  ( 0.7879377495398141029, 0.6157549048526801405, 0.000000000000000000 ) ) ;
#3637 = CIRCLE ( 'NONE', #3509, 6.930657474112426719 ) ;
#3639 = PERSON_AND_ORGANIZATION_ROLE ( 'classification_officer' ) ;
#3640 = DIRECTION ( 'NONE',  ( 0.7879377495398141029, 0.6157549048526802515, 0.000000000000000000 ) ) ;
#3641 = CIRCLE ( 'NONE', #5213, 0.1523203157102364369 ) ;
#3642 = CARTESIAN_POINT ( 'NONE',  ( 1.528753255969025782, 1.853077197008292210, -0.02325729969694005292 ) ) ;
#3643 = DIRECTION ( 'NONE',  ( 1.000000000000000000, 0.000000000000000000, 0.000000000000000000 ) ) ;
#3644 = LINE ( 'NONE', #6059, #2534 ) ;
#3645 = ADVANCED_FACE ( 'NONE', ( #630, #3786 ), #2663, .F. ) ;
#3646 = ADVANCED_FACE ( 'NONE', ( #6291 ), #3064, .T. ) ;
#3647 = DIRECTION ( 'NONE',  ( -0.000000000000000000, -0.000000000000000000, 1.000000000000000000 ) ) ;
#3648 = CC_DESIGN_PERSON_AND_ORGANIZATION_ASSIGNMENT ( #5882, #4725, ( #3702 ) ) ;
#3649 = LINE ( 'NONE', #2445, #5329 ) ;
#3650 = ADVANCED_FACE ( 'NONE', ( #2590 ), #5120, .F. ) ;
#3651 = ADVANCED_FACE ( 'NONE', ( #4562 ), #3744, .T. ) ;
#3652 = DIRECTION ( 'NONE',  ( 0.6157549048526803626, -0.7879377495398141029, 0.000000000000000000 ) ) ;
#3653 = ORIENTED_EDGE ( 'NONE', *, *, #6091, .F. ) ;
#3654 = DIRECTION ( 'NONE',  ( -1.000000000000000000, -0.000000000000000000, -0.000000000000000000 ) ) ;
#3655 = DIRECTION ( 'NONE',  ( -0.7879377495371227003, -0.6157549048561240523, -4.372694539034060785E-12 ) ) ;
#3656 = CARTESIAN_POINT ( 'NONE',  ( 1.681711120206815346, 1.342581682021484424, 0.2165151474863769854 ) ) ;
#3657 = PERSON_AND_ORGANIZATION_ROLE ( 'creator' ) ;
#3658 = VERTEX_POINT ( 'NONE', #7622 ) ;
#3659 = FACE_OUTER_BOUND ( 'NONE', #2073, .T. ) ;
#3660 = DIRECTION ( 'NONE',  ( 0.4606913525677331367, 0.8875604078987031631, 0.000000000000000000 ) ) ;
#3661 = ORIENTED_EDGE ( 'NONE', *, *, #5849, .F. ) ;
#3662 = DIRECTION ( 'NONE',  ( 1.000000000000000000, 0.000000000000000000, 0.000000000000000000 ) ) ;
#3663 = VERTEX_POINT ( 'NONE', #3906 ) ;
#3664 = DIRECTION ( 'NONE',  ( 1.000000000000000000, 0.000000000000000000, 0.000000000000000000 ) ) ;
#3665 =( LENGTH_UNIT ( ) NAMED_UNIT ( * ) SI_UNIT ( $, .METRE. ) );
#3666 = CYLINDRICAL_SURFACE ( 'NONE', #8015, 0.2499999999999998057 ) ;
#3667 = DATE_TIME_ROLE ( 'classification_date' ) ;
#3668 = LINE ( 'NONE', #2465, #333 ) ;
#3669 = VERTEX_POINT ( 'NONE', #6935 ) ;
#3670 =( BOUNDED_SURFACE ( )  B_SPLINE_SURFACE ( 3, 2, ( 
 ( #3062, #2987, #2357 ),
 ( #7368, #8011, #4264 ),
 ( #5615, #6148, #520 ),
 ( #1799, #4914, #3023 ),
 ( #3722, #4301, #6231 ),
 ( #6796, #3554, #3684 ),
 ( #3113, #5956, #2482 ),
 ( #1871, #6875, #3307 ),
 ( #5198, #6309, #5027 ),
 ( #2522, #7605, #2077 ),
 ( #4542, #5735, #7697 ),
 ( #7531, #28, #110 ) ),
 .UNSPECIFIED., .F., .F., .F. ) 
 B_SPLINE_SURFACE_WITH_KNOTS ( ( 4, 2, 2, 2, 2, 4 ),
 ( 3, 3 ),
 ( 0.000000000000000000, 0.001554125582113249264, 0.002331188373169874005, 0.003108251164226498529, 0.004662376746339748010, 0.006216502328452997057 ),
 ( 0.000000000000000000, 1.000000000000000000 ),
 .UNSPECIFIED. ) 
 GEOMETRIC_REPRESENTATION_ITEM ( )  RATIONAL_B_SPLINE_SURFACE ( (
 ( 1.000000000000000000, 0.7071067811871933895, 1.000000000000000000),
 ( 1.000000000000000000, 0.7276057061276963722, 1.000000000000000000),
 ( 1.000000000000000000, 0.7554750547903839042, 1.000000000000000000),
 ( 1.000000000000000000, 0.8015396134353254265, 1.000000000000000000),
 ( 1.000000000000000000, 0.8174651680526996422, 1.000000000000000000),
 ( 1.000000000000000000, 0.8485784994800038561, 1.000000000000000000),
 ( 1.000000000000000000, 0.8638859094028720209, 1.000000000000000000),
 ( 1.000000000000000000, 0.9076931387944575658, 1.000000000000000000),
 ( 1.000000000000000000, 0.9340604879544870398, 1.000000000000000000),
 ( 1.000000000000000000, 0.9743637288758403292, 1.000000000000000000),
 ( 1.000000000000000000, 0.9885326174603896732, 1.000000000000000000),
 ( 1.000000000000000000, 0.9952915331365300711, 1.000000000000000000) ) ) 
 REPRESENTATION_ITEM ( '' )  SURFACE ( )  );
#3671 = ORIENTED_EDGE ( 'NONE', *, *, #3685, .T. ) ;
#3672 = ORIENTED_EDGE ( 'NONE', *, *, #2524, .T. ) ;
#3673 = DIRECTION ( 'NONE',  ( -0.7879377495398138809, -0.6157549048526805846, 0.000000000000000000 ) ) ;
#3674 = CARTESIAN_POINT ( 'NONE',  ( -1.855136387357835481, 0.9645206712600612464, -0.2959999999999997078 ) ) ;
#3675 = FACE_OUTER_BOUND ( 'NONE', #5403, .T. ) ;
#3676 = PERSON_AND_ORGANIZATION ( #4735, #6190 ) ;
#3677 = DIRECTION ( 'NONE',  ( 0.000000000000000000, 0.000000000000000000, 1.000000000000000000 ) ) ;
#3678 = DIRECTION ( 'NONE',  ( -0.000000000000000000, -0.000000000000000000, -1.000000000000000000 ) ) ;
#3679 = EDGE_LOOP ( 'NONE', ( #3957, #7644 ) ) ;
#3680 = CARTESIAN_POINT ( 'NONE',  ( 1.576888795949508149, 1.175023536331549767, 0.1861679426474743271 ) ) ;
#3681 = CARTESIAN_POINT ( 'NONE',  ( 1.353740795342265546, 0.002292344206094486941, -6.650588809979335118E-06 ) ) ;
#3682 = ORIENTED_EDGE ( 'NONE', *, *, #6952, .F. ) ;
#3683 = CARTESIAN_POINT ( 'NONE',  ( 0.000000000000000000, 0.6124999999999999334, 0.000000000000000000 ) ) ;
#3684 = CARTESIAN_POINT ( 'NONE',  ( 1.334519317039704056, 1.071954003771020236, -0.09828849750274241959 ) ) ;
#3685 = EDGE_CURVE ( 'NONE', #4537, #1200, #3208, .T. ) ;
#3686 = DIRECTION ( 'NONE',  ( 0.000000000000000000, -0.000000000000000000, 1.000000000000000000 ) ) ;
#3687 = ORIENTED_EDGE ( 'NONE', *, *, #6945, .F. ) ;
#3688 = EDGE_CURVE ( 'NONE', #577, #4011, #6338, .T. ) ;
#3689 = CARTESIAN_POINT ( 'NONE',  ( -0.1250000000000000000, 0.6250000000000000000, 0.03125000000000000000 ) ) ;
#3690 = MANIFOLD_SOLID_BREP ( 'Boss-Extrude7', #191 ) ;
#3691 = APPROVAL ( #5344, 'UNSPECIFIED' ) ;
#3692 = LOCAL_TIME ( 14, 45, 32.00000000000000000, #2881 ) ;
#3693 = LINE ( 'NONE', #3121, #1767 ) ;
#3694 = DIRECTION ( 'NONE',  ( 0.000000000000000000, 0.000000000000000000, -1.000000000000000000 ) ) ;
#3695 = PERSON_AND_ORGANIZATION ( #4735, #6190 ) ;
#3696 = ORIENTED_EDGE ( 'NONE', *, *, #74, .T. ) ;
#3697 = CARTESIAN_POINT ( 'NONE',  ( -4.882388066182508091, 5.670153330992292240, 0.03199999999999999373 ) ) ;
#3698 = LINE ( 'NONE', #6201, #4013 ) ;
#3699 = EDGE_LOOP ( 'NONE', ( #4507, #5661, #3396, #959 ) ) ;
#3700 = CARTESIAN_POINT ( 'NONE',  ( 0.6250000000000000000, -0.07812500000000001388, 0.07449999999999999678 ) ) ;
#3701 = CC_DESIGN_APPROVAL ( #1185, ( #4603 ) ) ;
#3702 = SECURITY_CLASSIFICATION ( '', '', #6041 ) ;
#3703 = AXIS2_PLACEMENT_3D ( 'NONE', #5978, #4087, #6588 ) ;
#3704 = CARTESIAN_POINT ( 'NONE',  ( 1.854779829072218833, 1.467068431075036372, 0.01092961263066827109 ) ) ;
#3705 = CARTESIAN_POINT ( 'NONE',  ( 0.2386870781737283065, -0.03125000000000000000, 0.000000000000000000 ) ) ;
#3706 = AXIS2_PLACEMENT_3D ( 'NONE', #3291, #5669, #45 ) ;
#3707 = LOCAL_TIME ( 14, 45, 32.00000000000000000, #1091 ) ;
#3708 = CARTESIAN_POINT ( 'NONE',  ( 3.672767723898985537, -8.314396374632453401, 0.1250000000000000000 ) ) ;
#3709 = VECTOR ( 'NONE', #5117, 39.37007874015748143 ) ;
#3710 = ORIENTED_EDGE ( 'NONE', *, *, #3088, .F. ) ;
#3711 = VERTEX_POINT ( 'NONE', #683 ) ;
#3712 = CARTESIAN_POINT ( 'NONE',  ( 0.1250000000000000000, 1.530808498934191509E-17, 0.2500000000000000000 ) ) ;
#3713 = CARTESIAN_POINT ( 'NONE',  ( 6.067840808230170246, 0.2405569712445295161, 0.1850000000000003586 ) ) ;
#3714 = AXIS2_PLACEMENT_3D ( 'NONE', #1062, #3560, #4268 ) ;
#3715 = CARTESIAN_POINT ( 'NONE',  ( -0.03125000000000000000, 0.000000000000000000, 0.1162848326531996102 ) ) ;
#3716 = SHAPE_DEFINITION_REPRESENTATION ( #5462, #2298 ) ;
#3717 = CARTESIAN_POINT ( 'NONE',  ( 6.067840808230170246, 0.2405569712445295161, 5.393636709996481038 ) ) ;
#3718 = LINE ( 'NONE', #8002, #4260 ) ;
#3719 = CARTESIAN_POINT ( 'NONE',  ( 1.724226450181035597, 1.288377220358824182, 0.1823870340488806252 ) ) ;
#3720 = AXIS2_PLACEMENT_3D ( 'NONE', #3578, #2966, #4818 ) ;
#3721 = CARTESIAN_POINT ( 'NONE',  ( -0.02822771919328412663, 0.03615965030273324970, 0.1250000000000000000 ) ) ;
#3722 = CARTESIAN_POINT ( 'NONE',  ( 1.300898271301138331, 1.089340557784379770, -0.1081788068622108884 ) ) ;
#3723 = AXIS2_PLACEMENT_3D ( 'NONE', #7120, #146, #5105 ) ;
#3724 = AXIS2_PLACEMENT_3D ( 'NONE', #7694, #4614, #5732 ) ;
#3725 = CARTESIAN_POINT ( 'NONE',  ( 1.838053356874555622, 1.483773278494235015, 0.04018154866381434126 ) ) ;
#3726 = VERTEX_POINT ( 'NONE', #4457 ) ;
#3727 = DIRECTION ( 'NONE',  ( 1.000000000000000000, 0.000000000000000000, -0.000000000000000000 ) ) ;
#3728 = CIRCLE ( 'NONE', #7390, 0.3045082206899650812 ) ;
#3729 = B_SPLINE_CURVE_WITH_KNOTS ( 'NONE', 3,
 ( #4125, #6626, #6017, #2890 ),
 .UNSPECIFIED., .F., .F.,
 ( 4, 4 ),
 ( 0.9793902746300136020, 0.9794065391376511887 ),
 .UNSPECIFIED. ) ;
#3730 = ORIENTED_EDGE ( 'NONE', *, *, #1223, .F. ) ;
#3731 = CARTESIAN_POINT ( 'NONE',  ( 0.000000000000000000, 0.000000000000000000, 0.1250000000000000278 ) ) ;
#3732 = CARTESIAN_POINT ( 'NONE',  ( -0.06999999999999996503, -0.03125000000000000000, 0.8125000000000000000 ) ) ;
#3733 = CALENDAR_DATE ( 2026, 9, 10 ) ;
#3734 = VERTEX_POINT ( 'NONE', #2112 ) ;
#3735 = CARTESIAN_POINT ( 'NONE',  ( 1.994799250004547719, 1.182494687089567620, -0.1039999999999998703 ) ) ;
#3736 = CIRCLE ( 'NONE', #1242, 0.1875000000000000278 ) ;
#3737 = AXIS2_PLACEMENT_3D ( 'NONE', #1214, #1870, #3806 ) ;
#3738 = CARTESIAN_POINT ( 'NONE',  ( -1.411841654243101596, 0.8435981834898315102, 0.1250000000000000000 ) ) ;
#3739 = ADVANCED_FACE ( 'NONE', ( #3352 ), #1451, .T. ) ;
#3740 = ORIENTED_EDGE ( 'NONE', *, *, #1784, .T. ) ;
#3741 = CIRCLE ( 'NONE', #1508, 9.124497838702110286 ) ;
#3742 = DIRECTION ( 'NONE',  ( 0.000000000000000000, -0.000000000000000000, 1.000000000000000000 ) ) ;
#3743 = CARTESIAN_POINT ( 'NONE',  ( -4.715766759065554758, -0.9913700615931539950, -0.3289853186479057556 ) ) ;
#3744 = CYLINDRICAL_SURFACE ( 'NONE', #314, 0.03199999999999994515 ) ;
#3745 = SECURITY_CLASSIFICATION_LEVEL ( 'unclassified' ) ;
#3746 = CC_DESIGN_DATE_AND_TIME_ASSIGNMENT ( #4863, #2391, ( #7233 ) ) ;
#3747 = CARTESIAN_POINT ( 'NONE',  ( -1.045359630492886938, -0.7381809969516824887, 0.2465270810310471739 ) ) ;
#3748 = ADVANCED_FACE ( 'NONE', ( #143 ), #2030, .T. ) ;
#3749 = ORIENTED_EDGE ( 'NONE', *, *, #4450, .T. ) ;
#3750 = AXIS2_PLACEMENT_3D ( 'NONE', #6357, #3858, #6286 ) ;
#3751 = CIRCLE ( 'NONE', #4669, 0.01652128394798136474 ) ;
#3752 = AXIS2_PLACEMENT_3D ( 'NONE', #3626, #5054, #6777 ) ;
#3753 = ORIENTED_EDGE ( 'NONE', *, *, #1784, .F. ) ;
#3754 = CARTESIAN_POINT ( 'NONE',  ( 1.278468178840724834, 1.054204894366048473, -0.03540237177934978802 ) ) ;
#3755 = AXIS2_PLACEMENT_3D ( 'NONE', #7781, #2128, #7819 ) ;
#3756 = CARTESIAN_POINT ( 'NONE',  ( -6.420602001755994159, -1.404684638105634820, 0.3125000000000000000 ) ) ;
#3757 = DIRECTION ( 'NONE',  ( 0.6157549048526802515, -0.7879377495398142139, 0.000000000000000000 ) ) ;
#3758 = DATE_AND_TIME ( #1786, #6839 ) ;
#3760 = MANIFOLD_SOLID_BREP ( 'LPattern1', #2290 ) ;
#3759 = CARTESIAN_POINT ( 'NONE',  ( -0.6570132742846659379, -0.6068321365170168402, 0.2179999999999999993 ) ) ;
#3761 = LINE ( 'NONE', #7405, #718 ) ;
#3762 = ORIENTED_EDGE ( 'NONE', *, *, #6152, .F. ) ;
#3763 = CIRCLE ( 'NONE', #6519, 0.2515937209583816725 ) ;
#3764 = CIRCLE ( 'NONE', #2971, 0.1255000000000000282 ) ;
#3765 = ORIENTED_EDGE ( 'NONE', *, *, #669, .F. ) ;
#3766 = TOROIDAL_SURFACE ( 'NONE', #5205, 0.2704878104020024265, 0.03200000000000000067 ) ;
#3767 = AXIS2_PLACEMENT_3D ( 'NONE', #3458, #2150, #5965 ) ;
#3768 = ORIENTED_EDGE ( 'NONE', *, *, #1141, .T. ) ;
#3769 = DIRECTION ( 'NONE',  ( 0.000000000000000000, 0.000000000000000000, -1.000000000000000000 ) ) ;
#3770 = DIRECTION ( 'NONE',  ( -0.000000000000000000, -0.000000000000000000, -1.000000000000000000 ) ) ;
#3771 = DIRECTION ( 'NONE',  ( -0.4606913525677331367, -0.8875604078987031631, -0.000000000000000000 ) ) ;
#3772 = CIRCLE ( 'NONE', #1647, 0.03200000000000007006 ) ;
#3773 = FACE_OUTER_BOUND ( 'NONE', #4785, .T. ) ;
#3774 = CIRCLE ( 'NONE', #3485, 0.1250000000000000000 ) ;
#3775 = ORIENTED_EDGE ( 'NONE', *, *, #3488, .T. ) ;
#3776 = PLANE ( 'NONE',  #856 ) ;
#3777 = CYLINDRICAL_SURFACE ( 'NONE', #493, 0.2499400561648078278 ) ;
#3778 = PERSON_AND_ORGANIZATION_ROLE ( 'creator' ) ;
#3779 = VERTEX_POINT ( 'NONE', #4573 ) ;
#3780 = CARTESIAN_POINT ( 'NONE',  ( -0.1249999999999999445, 0.03125000000000000000, 0.06250000000000000000 ) ) ;
#3781 = CARTESIAN_POINT ( 'NONE',  ( -1.200653967786500020, -0.2165511910659388140, 0.2437698526464839588 ) ) ;
#3782 = VERTEX_POINT ( 'NONE', #3958 ) ;
#3783 = CARTESIAN_POINT ( 'NONE',  ( 1.532760465343473877, 1.242737084437108841, 0.2356017578317803340 ) ) ;
#3784 = LINE ( 'NONE', #6128, #1791 ) ;
#3785 = CARTESIAN_POINT ( 'NONE',  ( -2.290684594132797791, -0.9654407352564655653, 0.3377670380269011674 ) ) ;
#3786 = FACE_BOUND ( 'NONE', #5102, .T. ) ;
#3787 = APPROVAL_ROLE ( '' ) ;
#3788 = EDGE_CURVE ( 'NONE', #7457, #7619, #7255, .T. ) ;
#3789 = CARTESIAN_POINT ( 'NONE',  ( 0.1743677072153199392, -0.4209564106690024676, 0.1250000000000000000 ) ) ;
#3790 = ADVANCED_FACE ( 'NONE', ( #7643 ), #979, .T. ) ;
#3791 = EDGE_CURVE ( 'NONE', #6526, #1231, #4247, .T. ) ;
#3792 = ORIENTED_EDGE ( 'NONE', *, *, #3403, .F. ) ;
#3793 = CC_DESIGN_PERSON_AND_ORGANIZATION_ASSIGNMENT ( #7065, #674, ( #3498 ) ) ;
#3794 = ADVANCED_FACE ( 'NONE', ( #6953 ), #6462, .T. ) ;
#3795 = ORIENTED_EDGE ( 'NONE', *, *, #22, .T. ) ;
#3796 = EDGE_LOOP ( 'NONE', ( #3710, #3320, #6287, #309 ) ) ;
#3797 = EDGE_CURVE ( 'NONE', #5277, #5561, #2806, .T. ) ;
#3798 = DIRECTION ( 'NONE',  ( 0.000000000000000000, 1.000000000000000000, 0.000000000000000000 ) ) ;
#3799 = DIRECTION ( 'NONE',  ( -0.6568496200222102566, 0.7540216022612866720, 0.000000000000000000 ) ) ;
#3800 = CARTESIAN_POINT ( 'NONE',  ( 1.652539028737726179, 1.219618926967090289, -0.1039999999999998703 ) ) ;
#3801 = APPROVAL_DATE_TIME ( #757, #2036 ) ;
#3802 = CARTESIAN_POINT ( 'NONE',  ( -1.855136387357835481, 0.9645206712600612464, 0.1339999999999995361 ) ) ;
#3803 = DIRECTION ( 'NONE',  ( -1.000000000000000000, 0.000000000000000000, 0.000000000000000000 ) ) ;
#3804 = ORIENTED_EDGE ( 'NONE', *, *, #4340, .T. ) ;
#3805 = ORIENTED_EDGE ( 'NONE', *, *, #2287, .T. ) ;
#3806 = DIRECTION ( 'NONE',  ( -0.2873478855663426645, 0.000000000000000000, 0.9578262852211522071 ) ) ;
#3807 = DIRECTION ( 'NONE',  ( 0.04906492035527430795, -0.9987955914953422498, 0.000000000000000000 ) ) ;
#3808 = CARTESIAN_POINT ( 'NONE',  ( 1.844772722119052411, 1.489667545232676860, 0.02056656897901768324 ) ) ;
#3809 = VERTEX_POINT ( 'NONE', #3303 ) ;
#3810 = DIRECTION ( 'NONE',  ( 0.000000000000000000, -1.000000000000000000, 0.000000000000000000 ) ) ;
#3811 = ORIENTED_EDGE ( 'NONE', *, *, #4943, .T. ) ;
#3812 = VERTEX_POINT ( 'NONE', #5237 ) ;
#3813 = DIRECTION ( 'NONE',  ( 0.000000000000000000, 0.000000000000000000, 1.000000000000000000 ) ) ;
#3814 = CARTESIAN_POINT ( 'NONE',  ( 1.536996473475150671, 1.850194254988873244, -0.04789697820840163600 ) ) ;
#3815 = CALENDAR_DATE ( 2026, 9, 10 ) ;
#3816 = EDGE_LOOP ( 'NONE', ( #1961, #7972, #7829, #3551, #7119, #3856, #6187, #2947 ) ) ;
#3817 = LINE ( 'NONE', #7614, #3882 ) ;
#3818 = DIRECTION ( 'NONE',  ( 0.000000000000000000, 0.000000000000000000, -1.000000000000000000 ) ) ;
#3819 = LINE ( 'NONE', #5709, #5410 ) ;
#3820 = CARTESIAN_POINT ( 'NONE',  ( 1.782489676200804229, 1.410020151375938946, 0.1439750967038709029 ) ) ;
#3821 = PERSON_AND_ORGANIZATION_ROLE ( 'design_owner' ) ;
#3822 = DIRECTION ( 'NONE',  ( -0.000000000000000000, -0.000000000000000000, -1.000000000000000000 ) ) ;
#3823 = CARTESIAN_POINT ( 'NONE',  ( 1.520244955686326449, 1.863329565020348300, -0.0002333994861012334227 ) ) ;
#3824 = EDGE_CURVE ( 'NONE', #3501, #2354, #6990, .T. ) ;
#3825 = EDGE_CURVE ( 'NONE', #695, #4364, #7125, .T. ) ;
#3826 = EDGE_LOOP ( 'NONE', ( #2992, #75, #4899, #5743, #5851 ) ) ;
#3827 = LOCAL_TIME ( 14, 45, 32.00000000000000000, #7964 ) ;
#3828 = ADVANCED_FACE ( 'NONE', ( #5144, #107 ), #2563, .T. ) ;
#3829 = DIRECTION ( 'NONE',  ( 0.2853335501257686646, -0.9584282785752022971, 0.000000000000000000 ) ) ;
#3830 = CALENDAR_DATE ( 2026, 9, 10 ) ;
#3831 = CARTESIAN_POINT ( 'NONE',  ( 1.536996473475150671, 1.850194254988873244, -0.04789697820840163600 ) ) ;
#3832 = DIRECTION ( 'NONE',  ( 0.2853335501257686646, -0.9584282785752022971, 0.000000000000000000 ) ) ;
#3833 = AXIS2_PLACEMENT_3D ( 'NONE', #2868, #2901, #990 ) ;
#3834 = EDGE_LOOP ( 'NONE', ( #7218, #3633 ) ) ;
#3835 = ADVANCED_FACE ( 'NONE', ( #2597 ), #7118, .F. ) ;
#3836 = EDGE_CURVE ( 'NONE', #7370, #4400, #5103, .T. ) ;
#3837 = ADVANCED_FACE ( 'NONE', ( #5072 ), #6380, .F. ) ;
#3838 = VECTOR ( 'NONE', #4384, 39.37007874015748143 ) ;
#3839 = EDGE_LOOP ( 'NONE', ( #4789, #902, #1523, #7038, #1315, #5363, #2596, #7215 ) ) ;
#3840 = DIRECTION ( 'NONE',  ( -0.000000000000000000, 1.000000000000000000, -0.000000000000000000 ) ) ;
#3841 = EDGE_LOOP ( 'NONE', ( #1135, #6772, #7398, #1570 ) ) ;
#3842 = CARTESIAN_POINT ( 'NONE',  ( 1.725050460137628194, 1.380013254716581761, 0.2019012614946010253 ) ) ;
#3843 = DIRECTION ( 'NONE',  ( -1.000000000000000000, 0.000000000000000000, 0.000000000000000000 ) ) ;
#3844 = CC_DESIGN_PERSON_AND_ORGANIZATION_ASSIGNMENT ( #8041, #4418, ( #4480 ) ) ;
#3845 = CARTESIAN_POINT ( 'NONE',  ( -0.9157629057885486867, 0.6051665869063995729, -0.09374999999999998612 ) ) ;
#3846 = EDGE_CURVE ( 'NONE', #6385, #297, #7072, .T. ) ;
#3847 = CIRCLE ( 'NONE', #6597, 0.1100000000000000006 ) ;
#3848 = DIRECTION ( 'NONE',  ( 1.000000000000000000, 0.000000000000000000, 0.000000000000000000 ) ) ;
#3849 = AXIS2_PLACEMENT_3D ( 'NONE', #7475, #6863, #15 ) ;
#3850 = VECTOR ( 'NONE', #2856, 39.37007874015748854 ) ;
#3851 = VERTEX_POINT ( 'NONE', #7845 ) ;
#3852 = DIRECTION ( 'NONE',  ( -1.000000000000000000, 0.000000000000000000, -0.000000000000000000 ) ) ;
#3853 = ADVANCED_BREP_SHAPE_REPRESENTATION ( '', ( #3760, #3555 ), #2122 ) ;
#3854 = DIRECTION ( 'NONE',  ( -0.7540216022612862279, 0.6568496200222107007, 0.000000000000000000 ) ) ;
#3855 = PERSON_AND_ORGANIZATION_ROLE ( 'creator' ) ;
#3856 = ORIENTED_EDGE ( 'NONE', *, *, #857, .F. ) ;
#3857 = CARTESIAN_POINT ( 'NONE',  ( 0.1000000000000000472, 0.03125000000000000000, 0.7124999999999989120 ) ) ;
#3858 = DIRECTION ( 'NONE',  ( 0.000000000000000000, 0.000000000000000000, -1.000000000000000000 ) ) ;
#3859 = LINE ( 'NONE', #815, #4755 ) ;
#3860 = VECTOR ( 'NONE', #1433, 39.37007874015748143 ) ;
#3861 = ADVANCED_BREP_SHAPE_REPRESENTATION ( '', ( #3690, #3555 ), #2249 ) ;
#3862 = LINE ( 'NONE', #7057, #3625 ) ;
#3863 = DIRECTION ( 'NONE',  ( 0.000000000000000000, 0.000000000000000000, 1.000000000000000000 ) ) ;
#3864 = CARTESIAN_POINT ( 'NONE',  ( 0.000000000000000000, 0.000000000000000000, 0.1250000000000000278 ) ) ;
#3865 = AXIS2_PLACEMENT_3D ( 'NONE', #5026, #7263, #6308 ) ;
#3866 = CARTESIAN_POINT ( 'NONE',  ( 1.640223930641419914, 1.235377681954054285, -0.08212881570848259982 ) ) ;
#3867 = CARTESIAN_POINT ( 'NONE',  ( 0.000000000000000000, 0.000000000000000000, 0.1250000000000000000 ) ) ;
#3868 = AXIS2_PLACEMENT_3D ( 'NONE', #2809, #4774, #7272 ) ;
#3869 = CARTESIAN_POINT ( 'NONE',  ( 0.000000000000000000, -0.03125000000000000000, 0.000000000000000000 ) ) ;
#3870 = DIRECTION ( 'NONE',  ( 0.6578909993250586785, 0.7531131608245041908, 0.000000000000000000 ) ) ;
#3871 = LINE ( 'NONE', #3296, #2949 ) ;
#3872 = VECTOR ( 'NONE', #3660, 39.37007874015748143 ) ;
#3873 = EDGE_CURVE ( 'NONE', #5314, #684, #7876, .T. ) ;
#3874 = ORIENTED_EDGE ( 'NONE', *, *, #523, .F. ) ;
#3875 = CIRCLE ( 'NONE', #2696, 0.2499999999999998057 ) ;
#3876 = ORIENTED_EDGE ( 'NONE', *, *, #4953, .T. ) ;
#3877 = DIRECTION ( 'NONE',  ( -0.000000000000000000, -0.000000000000000000, -1.000000000000000000 ) ) ;
#3878 = EDGE_LOOP ( 'NONE', ( #1915, #1675, #6928, #2459, #1385, #4336 ) ) ;
#3880 = DIRECTION ( 'NONE',  ( -0.000000000000000000, -1.000000000000000000, -0.000000000000000000 ) ) ;
#3879 = VECTOR ( 'NONE', #6963, 39.37007874015748143 ) ;
#3881 = CARTESIAN_POINT ( 'NONE',  ( 4.405984854984288823, -2.483262103238899954, 0.09374999999999998612 ) ) ;
#3882 = VECTOR ( 'NONE', #5775, 39.37007874015748143 ) ;
#3883 = CARTESIAN_POINT ( 'NONE',  ( -1.983451234524918227, 1.341543513548240529, 0.1339999999999995917 ) ) ;
#3884 = ADVANCED_FACE ( 'NONE', ( #2160 ), #4736, .T. ) ;
#3885 = EDGE_CURVE ( 'NONE', #7983, #2070, #5425, .T. ) ;
#3886 = FACE_OUTER_BOUND ( 'NONE', #532, .T. ) ;
#3887 = EDGE_CURVE ( 'NONE', #1539, #7153, #1656, .T. ) ;
#3888 = CIRCLE ( 'NONE', #92, 0.1150000000000000050 ) ;
#3889 = ORIENTED_EDGE ( 'NONE', *, *, #942, .F. ) ;
#3890 = CC_DESIGN_DATE_AND_TIME_ASSIGNMENT ( #1045, #4078, ( #448 ) ) ;
#3891 = EDGE_CURVE ( 'NONE', #6385, #5439, #355, .T. ) ;
#3892 = EDGE_LOOP ( 'NONE', ( #932, #2701 ) ) ;
#3893 = CARTESIAN_POINT ( 'NONE',  ( 1.823416444783682477, 1.453886705131341772, 0.09198493102659689724 ) ) ;
#3894 = ADVANCED_FACE ( 'NONE', ( #4123 ), #5321, .F. ) ;
#3895 = DIRECTION ( 'NONE',  ( 0.000000000000000000, 1.000000000000000000, 0.000000000000000000 ) ) ;
#3896 = PERSON_AND_ORGANIZATION ( #4735, #6190 ) ;
#3897 = VERTEX_POINT ( 'NONE', #3513 ) ;
#3898 = CARTESIAN_POINT ( 'NONE',  ( -0.09374999999999998612, 1.148106374200643401E-17, 0.09374999999999998612 ) ) ;
#3899 = AXIS2_PLACEMENT_3D ( 'NONE', #6727, #1444, #6031 ) ;
#3900 = APPLICATION_CONTEXT ( 'configuration controlled 3d designs of mechanical parts and assemblies' ) ;
#3901 = CIRCLE ( 'NONE', #6907, 0.03200000000000009781 ) ;
#3902 = CARTESIAN_POINT ( 'NONE',  ( -1.197335310760672789, -0.2276984772474723306, 0.2492042935900711242 ) ) ;
#3903 = VERTEX_POINT ( 'NONE', #4084 ) ;
#3904 = DIRECTION ( 'NONE',  ( -0.6578909993250587895, -0.7531131608245040798, 0.000000000000000000 ) ) ;
#3905 = CARTESIAN_POINT ( 'NONE',  ( 0.09374999999999998612, 0.000000000000000000, 0.09374999999999998612 ) ) ;
#3906 = CARTESIAN_POINT ( 'NONE',  ( 0.1000000000000000472, -0.03125000000000000000, 0.06250000000000000000 ) ) ;
#3907 = CARTESIAN_POINT ( 'NONE',  ( 1.275565605498405253, -0.08258253728086821510, 0.1850000000000003586 ) ) ;
#3908 = DIRECTION ( 'NONE',  ( 0.000000000000000000, 0.000000000000000000, 1.000000000000000000 ) ) ;
#3909 = EDGE_LOOP ( 'NONE', ( #6781, #4716, #5310 ) ) ;
#3910 = LINE ( 'NONE', #4522, #6960 ) ;
#3911 = CARTESIAN_POINT ( 'NONE',  ( -0.06250000000000000000, 0.000000000000000000, 0.09374999999999998612 ) ) ;
#3912 = APPROVAL_STATUS ( 'not_yet_approved' ) ;
#3913 = CARTESIAN_POINT ( 'NONE',  ( 0.1000000000000000472, 0.03125000000000000000, 0.8125000000000000000 ) ) ;
#3914 = DIRECTION ( 'NONE',  ( -0.000000000000000000, -0.000000000000000000, -1.000000000000000000 ) ) ;
#3915 = ORIENTED_EDGE ( 'NONE', *, *, #4117, .T. ) ;
#3916 = ORIENTED_EDGE ( 'NONE', *, *, #7699, .T. ) ;
#3917 = ORIENTED_EDGE ( 'NONE', *, *, #6499, .F. ) ;
#3918 = DIRECTION ( 'NONE',  ( 1.000000000000000000, 0.000000000000000000, 0.000000000000000000 ) ) ;
#3919 = VERTEX_POINT ( 'NONE', #4825 ) ;
#3920 = CARTESIAN_POINT ( 'NONE',  ( 1.676936960580814651, 1.351834804519730815, 0.2274697013873200890 ) ) ;
#3921 = CARTESIAN_POINT ( 'NONE',  ( 0.9690125299525020885, 0.8529848947786566882, 0.2500000000000000000 ) ) ;
#3922 = DIRECTION ( 'NONE',  ( -1.000000000000000000, 0.000000000000000000, 0.000000000000000000 ) ) ;
#3923 = DIRECTION ( 'NONE',  ( -1.000000000000000000, 0.000000000000000000, 0.000000000000000000 ) ) ;
#3924 =( BOUNDED_CURVE ( )  B_SPLINE_CURVE ( 3, ( #7770, #5324, #2163, #4740 ),
 .UNSPECIFIED., .F., .T. ) 
 B_SPLINE_CURVE_WITH_KNOTS ( ( 4, 4 ),
 ( 1.570796326794897668, 2.774242905800009318 ),
 .UNSPECIFIED. ) 
 CURVE ( )  GEOMETRIC_REPRESENTATION_ITEM ( )  RATIONAL_B_SPLINE_CURVE ( ( 1.000000000000000000, 0.8829075649559229300, 0.8829075649559229300, 1.000000000000000000 ) ) 
 REPRESENTATION_ITEM ( '' )  );
#3925 = EDGE_CURVE ( 'NONE', #3222, #112, #4166, .T. ) ;
#3926 = ADVANCED_FACE ( 'NONE', ( #5971 ), #7199, .F. ) ;
#3927 = CARTESIAN_POINT ( 'NONE',  ( 1.508907770781040547, 1.868855936767433779, 0.03336486358077169617 ) ) ;
#3928 = CARTESIAN_POINT ( 'NONE',  ( -1.763177565995707630, 1.070083551578369763, 0.1339999999999995361 ) ) ;
#3929 = CALENDAR_DATE ( 2026, 9, 10 ) ;
#3930 = CARTESIAN_POINT ( 'NONE',  ( 0.06250000000000000000, 7.654042494670957545E-18, -0.6537499999999999423 ) ) ;
#3931 = DIRECTION ( 'NONE',  ( 1.000000000000000000, 0.000000000000000000, 0.000000000000000000 ) ) ;
#3932 = DIRECTION ( 'NONE',  ( 0.6157549048526804736, -0.7879377495398138809, 0.000000000000000000 ) ) ;
#3933 = VERTEX_POINT ( 'NONE', #3542 ) ;
#3934 = LINE ( 'NONE', #2610, #3709 ) ;
#3935 = APPROVAL ( #2408, 'UNSPECIFIED' ) ;
#3936 = EDGE_CURVE ( 'NONE', #5830, #6526, #449, .T. ) ;
#3937 = DIRECTION ( 'NONE',  ( 0.000000000000000000, -1.000000000000000000, 0.000000000000000000 ) ) ;
#3938 = DIRECTION ( 'NONE',  ( 0.000000000000000000, 0.000000000000000000, -1.000000000000000000 ) ) ;
#3939 = PERSON_AND_ORGANIZATION ( #4735, #6190 ) ;
#3940 = ORIENTED_EDGE ( 'NONE', *, *, #6397, .F. ) ;
#3941 = CARTESIAN_POINT ( 'NONE',  ( 1.877293513487986676, 1.420642010912031683, -0.07224819784990933746 ) ) ;
#3942 = CARTESIAN_POINT ( 'NONE',  ( 1.434855324240962071, 1.174358127631301540, 0.2233288069132987330 ) ) ;
#3943 = CC_DESIGN_PERSON_AND_ORGANIZATION_ASSIGNMENT ( #3377, #1435, ( #7756 ) ) ;
#3944 = ORIENTED_EDGE ( 'NONE', *, *, #7041, .F. ) ;
#3945 = LINE ( 'NONE', #5061, #2117 ) ;
#3946 = VERTEX_POINT ( 'NONE', #5931 ) ;
#3947 = CIRCLE ( 'NONE', #1594, 9.124497838702110286 ) ;
#3948 = DIRECTION ( 'NONE',  ( 0.7540216022612863389, -0.6568496200222107007, 0.000000000000000000 ) ) ;
#3949 = CALENDAR_DATE ( 2026, 9, 10 ) ;
#3950 = DIRECTION ( 'NONE',  ( -1.000000000000000000, 0.000000000000000000, 0.000000000000000000 ) ) ;
#3951 = DIRECTION ( 'NONE',  ( 1.000000000000000000, -1.821231995776175479E-16, 0.000000000000000000 ) ) ;
#3952 = EDGE_LOOP ( 'NONE', ( #2042, #291, #6339, #2504 ) ) ;
#3953 = VECTOR ( 'NONE', #6467, 39.37007874015748143 ) ;
#3954 = ORIENTED_EDGE ( 'NONE', *, *, #1311, .F. ) ;
#3955 = LOCAL_TIME ( 14, 45, 32.00000000000000000, #6354 ) ;
#3956 = VERTEX_POINT ( 'NONE', #307 ) ;
#3957 = ORIENTED_EDGE ( 'NONE', *, *, #6192, .T. ) ;
#3958 = CARTESIAN_POINT ( 'NONE',  ( -1.050138139902704104, -0.7221301030214424266, 0.000000000000000000 ) ) ;
#3959 = ORIENTED_EDGE ( 'NONE', *, *, #1040, .T. ) ;
#3960 = VECTOR ( 'NONE', #2460, 39.37007874015748143 ) ;
#3961 = CARTESIAN_POINT ( 'NONE',  ( 1.571814533976791495, 1.273076930690883124, 0.2372021369713644967 ) ) ;
#3962 = CARTESIAN_POINT ( 'NONE',  ( -0.1250000000000000000, 1.530808498934191509E-17, 0.000000000000000000 ) ) ;
#3963 = CARTESIAN_POINT ( 'NONE',  ( 0.1250000000000000000, 0.6250000000000000000, 0.000000000000000000 ) ) ;
#3964 = CARTESIAN_POINT ( 'NONE',  ( -0.9157629057885486867, 0.6051665869063995729, 0.09374999999999998612 ) ) ;
#3965 = ORIENTED_EDGE ( 'NONE', *, *, #3992, .T. ) ;
#3966 = CIRCLE ( 'NONE', #6199, 0.1250000000000000000 ) ;
#3967 = ORIENTED_EDGE ( 'NONE', *, *, #3492, .T. ) ;
#3968 = CARTESIAN_POINT ( 'NONE',  ( 1.359242672892850390, 1.751896166577295633, 0.2197878876622516298 ) ) ;
#3969 = CARTESIAN_POINT ( 'NONE',  ( 0.1250000000000000278, -0.03125000000000000000, 0.06250000000000000000 ) ) ;
#3970 = APPROVAL_STATUS ( 'not_yet_approved' ) ;
#3971 = VERTEX_POINT ( 'NONE', #2888 ) ;
#3972 = VECTOR ( 'NONE', #4876, 39.37007874015748854 ) ;
#3973 = CARTESIAN_POINT ( 'NONE',  ( 6.190240298342082781, 0.4584752965318059093, 0.1850000000000003586 ) ) ;
#3974 = CARTESIAN_POINT ( 'NONE',  ( -9.251037553912103917, -0.6017136928027502218, 0.3125000000000000000 ) ) ;
#3975 = ORIENTED_EDGE ( 'NONE', *, *, #5028, .T. ) ;
#3976 = DIRECTION ( 'NONE',  ( -0.000000000000000000, -0.000000000000000000, -1.000000000000000000 ) ) ;
#3977 = CIRCLE ( 'NONE', #6857, 0.2149999999999995803 ) ;
#3978 = AXIS2_PLACEMENT_3D ( 'NONE', #3457, #1532, #2263 ) ;
#3979 = CARTESIAN_POINT ( 'NONE',  ( 0.000000000000000000, -0.03125000000000000000, 0.000000000000000000 ) ) ;
#3980 = CARTESIAN_POINT ( 'NONE',  ( 1.260018307975525387, 1.633742302984368733, 0.2500000000000000000 ) ) ;
#3981 = DATE_AND_TIME ( #3281, #5671 ) ;
#3982 = ORIENTED_EDGE ( 'NONE', *, *, #5991, .T. ) ;
#3983 = EDGE_CURVE ( 'NONE', #4234, #7191, #2543, .T. ) ;
#3984 = CARTESIAN_POINT ( 'NONE',  ( 1.258616367985684104, -0.02482036785324303815, 0.1849999999999999978 ) ) ;
#3985 = VECTOR ( 'NONE', #4565, 39.37007874015748143 ) ;
#3986 = LOCAL_TIME ( 14, 45, 32.00000000000000000, #2347 ) ;
#3987 = AXIS2_PLACEMENT_3D ( 'NONE', #6256, #1901, #665 ) ;
#3988 = DIRECTION ( 'NONE',  ( -0.9595416650617119014, -0.2815666759589949275, 0.000000000000000000 ) ) ;
#3989 = EDGE_CURVE ( 'NONE', #4051, #1004, #1100, .T. ) ;
#3990 = EDGE_CURVE ( 'NONE', #4011, #2564, #3728, .T. ) ;
#3991 = EDGE_CURVE ( 'NONE', #774, #3622, #265, .T. ) ;
#3992 = EDGE_CURVE ( 'NONE', #6, #3812, #188, .T. ) ;
#3993 = AXIS2_PLACEMENT_3D ( 'NONE', #1250, #2980, #4906 ) ;
#3994 = AXIS2_PLACEMENT_3D ( 'NONE', #1681, #4713, #4842 ) ;
#3995 = VERTEX_POINT ( 'NONE', #4052 ) ;
#3996 = APPROVAL ( #4208, 'UNSPECIFIED' ) ;
#3997 = ADVANCED_FACE ( 'NONE', ( #934 ), #2814, .T. ) ;
#3998 = ORIENTED_EDGE ( 'NONE', *, *, #2780, .T. ) ;
#3999 = CARTESIAN_POINT ( 'NONE',  ( 0.8135394388129589816, 1.284829519251779573, 0.000000000000000000 ) ) ;
#4000 = FACE_OUTER_BOUND ( 'NONE', #2211, .T. ) ;
#4001 = DATE_AND_TIME ( #1611, #825 ) ;
#4002 = CARTESIAN_POINT ( 'NONE',  ( 0.000000000000000000, 0.03125000000000000000, 0.6646281645421511231 ) ) ;
#4003 = CARTESIAN_POINT ( 'NONE',  ( 1.859621461000523945, 1.475107775274728361, -0.006828021556016123858 ) ) ;
#4004 = ADVANCED_FACE ( 'NONE', ( #3466 ), #2547, .T. ) ;
#4005 = VERTEX_POINT ( 'NONE', #3754 ) ;
#4006 = ORIENTED_EDGE ( 'NONE', *, *, #3278, .T. ) ;
#4007 = VECTOR ( 'NONE', #7196, 39.37007874015748854 ) ;
#4008 = AXIS2_PLACEMENT_3D ( 'NONE', #1588, #4094, #2282 ) ;
#4009 = ORIENTED_EDGE ( 'NONE', *, *, #5191, .T. ) ;
#4010 = ORIENTED_EDGE ( 'NONE', *, *, #2780, .F. ) ;
#4011 = VERTEX_POINT ( 'NONE', #4250 ) ;
#4012 = DIRECTION ( 'NONE',  ( 0.000000000000000000, 1.000000000000000000, -0.000000000000000000 ) ) ;
#4013 = VECTOR ( 'NONE', #570, 39.37007874015748143 ) ;
#4014 = DESIGN_CONTEXT ( 'detailed design', #1950, 'design' ) ;
#4015 = ORIENTED_EDGE ( 'NONE', *, *, #4194, .F. ) ;
#4016 = CARTESIAN_POINT ( 'NONE',  ( 1.579309947762197686, 1.291120561748658302, 0.2500517076223078283 ) ) ;
#4017 = LINE ( 'NONE', #2732, #7022 ) ;
#4018 = CYLINDRICAL_SURFACE ( 'NONE', #4222, 0.1875000000000000278 ) ;
#4019 = DIRECTION ( 'NONE',  ( 1.000000000000000000, 0.000000000000000000, 0.000000000000000000 ) ) ;
#4020 = VECTOR ( 'NONE', #5255, 39.37007874015748143 ) ;
#4021 = ORIENTED_EDGE ( 'NONE', *, *, #5359, .F. ) ;
#4022 = AXIS2_PLACEMENT_3D ( 'NONE', #4026, #5289, #3406 ) ;
#4023 = AXIS2_PLACEMENT_3D ( 'NONE', #3006, #6208, #7508 ) ;
#4024 = PRODUCT ( 'Cleco, Handle, Pivoting', 'Cleco, Handle, Pivoting', '', ( #5558 ) ) ;
#4025 = CARTESIAN_POINT ( 'NONE',  ( 1.861435943104858604, 1.485749338168939726, -0.007975310270593111497 ) ) ;
#4026 = CARTESIAN_POINT ( 'NONE',  ( 1.723350842796532278, 1.129006085766179890, -0.1039999999999998703 ) ) ;
#4027 = CALENDAR_DATE ( 2026, 9, 10 ) ;
#4028 = FACE_OUTER_BOUND ( 'NONE', #6182, .T. ) ;
#4029 = LINE ( 'NONE', #323, #213 ) ;
#4030 = VECTOR ( 'NONE', #1834, 39.37007874015748143 ) ;
#4031 = CARTESIAN_POINT ( 'NONE',  ( -1.052129263295328521, 0.6378420796487936917, 0.1250000000000000000 ) ) ;
#4032 = DIRECTION ( 'NONE',  ( -0.6157549048526823610, 0.7879377495398123266, 0.000000000000000000 ) ) ;
#4033 = CIRCLE ( 'NONE', #100, 0.2500000000000000555 ) ;
#4034 = FACE_OUTER_BOUND ( 'NONE', #7227, .T. ) ;
#4035 = PERSON_AND_ORGANIZATION_ROLE ( 'design_supplier' ) ;
#4036 = EDGE_LOOP ( 'NONE', ( #1193, #3127, #4557, #7882 ) ) ;
#4037 = DIRECTION ( 'NONE',  ( 0.000000000000000000, 1.000000000000000000, 0.000000000000000000 ) ) ;
#4038 = CARTESIAN_POINT ( 'NONE',  ( 0.000000000000000000, 0.000000000000000000, -0.1250000000000000000 ) ) ;
#4039 = EDGE_LOOP ( 'NONE', ( #571, #559, #2810, #2497 ) ) ;
#4040 = CARTESIAN_POINT ( 'NONE',  ( -0.7707523566753868849, 1.573689170607686316, -0.2208252761660650376 ) ) ;
#4041 = ADVANCED_FACE ( 'NONE', ( #1780 ), #6218, .T. ) ;
#4042 = EDGE_CURVE ( 'NONE', #6252, #777, #4647, .T. ) ;
#4043 = DIRECTION ( 'NONE',  ( -0.000000000000000000, -1.000000000000000000, -0.000000000000000000 ) ) ;
#4044 = CARTESIAN_POINT ( 'NONE',  ( 1.244866787915867912, 1.068558539350931369, -0.06210292240210582571 ) ) ;
#4045 = COORDINATED_UNIVERSAL_TIME_OFFSET ( 0, 0, .AHEAD. ) ;
#4046 = CARTESIAN_POINT ( 'NONE',  ( 1.302790242782180918, 1.667167568704493341, -0.1039999999999998703 ) ) ;
#4047 = ORIENTED_EDGE ( 'NONE', *, *, #3536, .F. ) ;
#4048 = ORIENTED_EDGE ( 'NONE', *, *, #82, .F. ) ;
#4049 = ADVANCED_FACE ( 'NONE', ( #6263 ), #5511, .T. ) ;
#4050 = EDGE_CURVE ( 'NONE', #4005, #577, #5552, .T. ) ;
#4051 = VERTEX_POINT ( 'NONE', #3097 ) ;
#4052 = CARTESIAN_POINT ( 'NONE',  ( 0.1210307295689817542, 0.6124999999999999334, 0.03125000000000000000 ) ) ;
#4053 = ORIENTED_EDGE ( 'NONE', *, *, #823, .F. ) ;
#4054 = EDGE_CURVE ( 'NONE', #4355, #3734, #5306, .T. ) ;
#4055 = CARTESIAN_POINT ( 'NONE',  ( 0.03125000000000000000, 0.000000000000000000, -0.1106726592253027830 ) ) ;
#4056 = DIRECTION ( 'NONE',  ( -0.8680936205257663296, 0.4964005096718442922, 0.000000000000000000 ) ) ;
#4057 = DIRECTION ( 'NONE',  ( 1.000000000000000000, -0.000000000000000000, -0.000000000000000000 ) ) ;
#4058 = DIRECTION ( 'NONE',  ( -0.6574491177601826664, -0.5137810939865956605, 0.5511711576436982840 ) ) ;
#4059 = APPLICATION_CONTEXT ( 'configuration controlled 3d designs of mechanical parts and assemblies' ) ;
#4060 = CARTESIAN_POINT ( 'NONE',  ( 1.753265575557962253, 1.417851156428476589, 0.1719230015339517637 ) ) ;
#4061 = CARTESIAN_POINT ( 'NONE',  ( 2.054765106439577771, 0.7510910599158125978, -0.09374999999999998612 ) ) ;
#4062 = CARTESIAN_POINT ( 'NONE',  ( -0.1250000000000000000, 0.000000000000000000, 0.2500000000000000000 ) ) ;
#4063 = ORIENTED_EDGE ( 'NONE', *, *, #7583, .F. ) ;
#4064 = DIRECTION ( 'NONE',  ( -0.000000000000000000, -0.000000000000000000, 1.000000000000000000 ) ) ;
#4065 = DIRECTION ( 'NONE',  ( 0.000000000000000000, 0.000000000000000000, -1.000000000000000000 ) ) ;
#4066 = DIRECTION ( 'NONE',  ( 0.000000000000000000, 0.000000000000000000, 1.000000000000000000 ) ) ;
#4067 = APPLICATION_PROTOCOL_DEFINITION ( 'international standard', 'config_control_design', 1994, #4728 ) ;
#4068 = VERTEX_POINT ( 'NONE', #2433 ) ;
#4069 = CARTESIAN_POINT ( 'NONE',  ( 1.142655413120957197, 0.6307864494084283180, 0.000000000000000000 ) ) ;
#4070 = CARTESIAN_POINT ( 'NONE',  ( 1.452776126473085183, 1.185506347940141092, 0.2257575757574807884 ) ) ;
#4071 = ORIENTED_EDGE ( 'NONE', *, *, #2330, .F. ) ;
#4072 = VERTEX_POINT ( 'NONE', #4941 ) ;
#4073 = ORIENTED_EDGE ( 'NONE', *, *, #2422, .T. ) ;
#4074 =( CONVERSION_BASED_UNIT ( 'INCH', #7152 ) LENGTH_UNIT ( ) NAMED_UNIT ( #2530 ) );
#4075 = ORIENTED_EDGE ( 'NONE', *, *, #4117, .F. ) ;
#4076 = FACE_OUTER_BOUND ( 'NONE', #4853, .T. ) ;
#4077 = CARTESIAN_POINT ( 'NONE',  ( 1.431357298810053358, 1.177565498724364446, 0.2499999999999698019 ) ) ;
#4078 = DATE_TIME_ROLE ( 'classification_date' ) ;
#4079 = CARTESIAN_POINT ( 'NONE',  ( 1.853159119997093596, 1.491110577246867797, -1.005434777941619967E-16 ) ) ;
#4080 = ORIENTED_EDGE ( 'NONE', *, *, #8026, .F. ) ;
#4081 = VERTEX_POINT ( 'NONE', #4288 ) ;
#4082 = ORIENTED_EDGE ( 'NONE', *, *, #5583, .F. ) ;
#4083 = PRODUCT_DEFINITION_FORMATION_WITH_SPECIFIED_SOURCE ( 'ANY', '', #3286, .NOT_KNOWN. ) ;
#4084 = CARTESIAN_POINT ( 'NONE',  ( -1.499610808650658100, -1.013166758633947007, 0.3125000000000000000 ) ) ;
#4085 = LINE ( 'NONE', #7320, #4375 ) ;
#4086 = PLANE ( 'NONE',  #2702 ) ;
#4087 = DIRECTION ( 'NONE',  ( 0.000000000000000000, 0.000000000000000000, -1.000000000000000000 ) ) ;
#4088 = DIRECTION ( 'NONE',  ( -0.000000000000000000, -1.000000000000000000, -0.000000000000000000 ) ) ;
#4089 = CC_DESIGN_APPROVAL ( #3146, ( #7867 ) ) ;
#4090 = EDGE_CURVE ( 'NONE', #5293, #4149, #1759, .T. ) ;
#4091 = EDGE_CURVE ( 'NONE', #365, #2424, #1106, .T. ) ;
#4092 = EDGE_LOOP ( 'NONE', ( #4378, #3805, #6186, #6237 ) ) ;
#4093 = APPROVAL_PERSON_ORGANIZATION ( #1702, #3996, #7656 ) ;
#4094 = DIRECTION ( 'NONE',  ( -0.6157549048526802515, 0.7879377495398139919, -0.000000000000000000 ) ) ;
#4095 = APPROVAL_PERSON_ORGANIZATION ( #3175, #5598, #715 ) ;
#4096 = PRODUCT_RELATED_PRODUCT_CATEGORY ( 'detail', '', ( #4024 ) ) ;
#4097 = DIRECTION ( 'NONE',  ( -0.7879377495398137699, -0.6157549048526804736, 9.031266384036010773E-16 ) ) ;
#4098 = ADVANCED_FACE ( 'NONE', ( #3587 ), #7136, .F. ) ;
#4099 = DIRECTION ( 'NONE',  ( 0.04906492035527816598, -0.9987955914953420278, 0.000000000000000000 ) ) ;
#4100 = ORIENTED_EDGE ( 'NONE', *, *, #6198, .F. ) ;
#4101 = VECTOR ( 'NONE', #407, 39.37007874015748143 ) ;
#4102 = CARTESIAN_POINT ( 'NONE',  ( 0.000000000000000000, 0.000000000000000000, 0.000000000000000000 ) ) ;
#4103 = LINE ( 'NONE', #4639, #1932 ) ;
#4104 = DATE_AND_TIME ( #7058, #5118 ) ;
#4105 = VERTEX_POINT ( 'NONE', #4860 ) ;
#4106 = ORIENTED_EDGE ( 'NONE', *, *, #5298, .F. ) ;
#4107 = CARTESIAN_POINT ( 'NONE',  ( 0.3425853749674607762, -0.3527052086967336075, 0.2385123635927634544 ) ) ;
#4108 = CARTESIAN_POINT ( 'NONE',  ( 1.447554089980937819, 1.218396913779240753, 0.2500000000000000000 ) ) ;
#4109 = ORIENTED_EDGE ( 'NONE', *, *, #2135, .T. ) ;
#4110 = AXIS2_PLACEMENT_3D ( 'NONE', #910, #1625, #2735 ) ;
#4111 = ORIENTED_EDGE ( 'NONE', *, *, #1777, .T. ) ;
#4112 = VECTOR ( 'NONE', #1701, 39.37007874015748143 ) ;
#4113 = ORIENTED_EDGE ( 'NONE', *, *, #8079, .T. ) ;
#4114 = CARTESIAN_POINT ( 'NONE',  ( 1.863737827646003042, 1.449134593498074386, -0.03116755751364449697 ) ) ;
#4115 = VECTOR ( 'NONE', #7915, 39.37007874015748143 ) ;
#4116 = CARTESIAN_POINT ( 'NONE',  ( -1.041991915560238624, -0.7494930674187111341, 0.01525612839587352394 ) ) ;
#4117 = EDGE_CURVE ( 'NONE', #4706, #3574, #1202, .T. ) ;
#4118 = CALENDAR_DATE ( 2026, 9, 10 ) ;
#4119 = CARTESIAN_POINT ( 'NONE',  ( -0.1250000000000000000, 0.6250000000000000000, 0.03125000000000000000 ) ) ;
#4120 = ORIENTED_EDGE ( 'NONE', *, *, #6697, .T. ) ;
#4121 = ORIENTED_EDGE ( 'NONE', *, *, #1311, .T. ) ;
#4122 = LOCAL_TIME ( 14, 45, 32.00000000000000000, #4318 ) ;
#4123 = FACE_OUTER_BOUND ( 'NONE', #3145, .T. ) ;
#4124 = FACE_OUTER_BOUND ( 'NONE', #1849, .T. ) ;
#4125 = CARTESIAN_POINT ( 'NONE',  ( 1.353816004522938599, 0.002313473902802895728, -0.1250000000000000278 ) ) ;
#4126 = VERTEX_POINT ( 'NONE', #509 ) ;
#4127 = EDGE_CURVE ( 'NONE', #3995, #4366, #2470, .T. ) ;
#4128 = CIRCLE ( 'NONE', #7267, 0.1250000000000000000 ) ;
#4129 = DIRECTION ( 'NONE',  ( 0.000000000000000000, 0.000000000000000000, 1.000000000000000000 ) ) ;
#4130 = DIRECTION ( 'NONE',  ( -0.6568496200222102566, 0.7540216022612866720, 0.000000000000000000 ) ) ;
#4131 = AXIS2_PLACEMENT_3D ( 'NONE', #5184, #7600, #4606 ) ;
#4132 = ORIENTED_EDGE ( 'NONE', *, *, #4230, .T. ) ;
#4133 = DIRECTION ( 'NONE',  ( 1.000000000000000000, 7.087526815720798773E-15, 0.000000000000000000 ) ) ;
#4134 = CARTESIAN_POINT ( 'NONE',  ( 0.6250000000000000000, -0.07812500000000001388, 0.07449999999999999678 ) ) ;
#4135 = EDGE_CURVE ( 'NONE', #4276, #6720, #1902, .T. ) ;
#4136 = ADVANCED_FACE ( 'NONE', ( #13 ), #2509, .T. ) ;
#4137 = DIRECTION ( 'NONE',  ( -0.000000000000000000, -0.000000000000000000, -1.000000000000000000 ) ) ;
#4138 = AXIS2_PLACEMENT_3D ( 'NONE', #3076, #5582, #8064 ) ;
#4139 = ORIENTED_EDGE ( 'NONE', *, *, #634, .T. ) ;
#4140 = FACE_OUTER_BOUND ( 'NONE', #3816, .T. ) ;
#4141 = CIRCLE ( 'NONE', #1253, 0.4024878104020025438 ) ;
#4142 = EDGE_CURVE ( 'NONE', #4722, #3812, #3050, .T. ) ;
#4143 = EDGE_CURVE ( 'NONE', #4623, #3222, #4258, .T. ) ;
#4144 = TOROIDAL_SURFACE ( 'NONE', #471, 0.2812500000000000000, 0.03125000000000000000 ) ;
#4145 = ORGANIZATION ( 'NAUO-ORG2', 'UNSPECIFIED', 'UNSPECIFIED' ) ;
#4146 = CARTESIAN_POINT ( 'NONE',  ( -1.196131363052349350, -0.2317425075729434292, -7.414317267960868635E-18 ) ) ;
#4147 = DIRECTION ( 'NONE',  ( 0.000000000000000000, 0.000000000000000000, -1.000000000000000000 ) ) ;
#4148 = DATE_AND_TIME ( #1639, #6444 ) ;
#4149 = VERTEX_POINT ( 'NONE', #6909 ) ;
#4150 = DIRECTION ( 'NONE',  ( -0.000000000000000000, -1.000000000000000000, -0.000000000000000000 ) ) ;
#4151 = TOROIDAL_SURFACE ( 'NONE', #2310, 0.1255000000000000282, 0.06199999999999999956 ) ;
#4152 = AXIS2_PLACEMENT_3D ( 'NONE', #2661, #782, #6437 ) ;
#4153 = DIRECTION ( 'NONE',  ( 1.000000000000000000, 0.000000000000000000, 0.000000000000000000 ) ) ;
#4154 = PRODUCT_DEFINITION_SHAPE ( 'NONE', 'NONE',  #8098 ) ;
#4155 = CARTESIAN_POINT ( 'NONE',  ( 1.527344374864917365, 1.250631131126433537, 0.2500000000000000555 ) ) ;
#4156 = AXIS2_PLACEMENT_3D ( 'NONE', #7948, #2340, #5271 ) ;
#4157 = ORIENTED_EDGE ( 'NONE', *, *, #1773, .F. ) ;
#4158 = AXIS2_PLACEMENT_3D ( 'NONE', #5556, #2388, #4901 ) ;
#4159 = ORIENTED_EDGE ( 'NONE', *, *, #4377, .T. ) ;
#4160 = DIRECTION ( 'NONE',  ( 0.000000000000000000, 0.000000000000000000, -1.000000000000000000 ) ) ;
#4161 = CARTESIAN_POINT ( 'NONE',  ( 1.437142212821967968, 1.212327995214759424, 0.2500000000000000000 ) ) ;
#4162 = APPROVAL_STATUS ( 'not_yet_approved' ) ;
#4163 = DIRECTION ( 'NONE',  ( 0.000000000000000000, 0.000000000000000000, 1.000000000000000000 ) ) ;
#4164 = AXIS2_PLACEMENT_3D ( 'NONE', #7464, #6847, #1229 ) ;
#4165 = TOROIDAL_SURFACE ( 'NONE', #3767, 0.4024878104020024328, 0.1000000000000000056 ) ;
#4166 = LINE ( 'NONE', #6050, #4898 ) ;
#4167 = CARTESIAN_POINT ( 'NONE',  ( -1.023858060246952029, -0.8104042351526981047, 0.3125000000000000000 ) ) ;
#4168 = PERSON_AND_ORGANIZATION ( #4735, #6190 ) ;
#4169 = DIRECTION ( 'NONE',  ( -0.000000000000000000, -1.000000000000000000, -0.000000000000000000 ) ) ;
#4170 = ORIENTED_EDGE ( 'NONE', *, *, #6543, .T. ) ;
#4171 = EDGE_LOOP ( 'NONE', ( #3304, #5203, #6129, #5101, #6969, #2019 ) ) ;
#4172 = CARTESIAN_POINT ( 'NONE',  ( 1.495975307881522998, 1.195556502892835660, 0.1713108456322826045 ) ) ;
#4173 = LINE ( 'NONE', #7968, #5290 ) ;
#4174 = VERTEX_POINT ( 'NONE', #671 ) ;
#4175 = FACE_OUTER_BOUND ( 'NONE', #5807, .T. ) ;
#4176 = DIRECTION ( 'NONE',  ( 0.000000000000000000, -1.000000000000000000, 0.000000000000000000 ) ) ;
#4177 = CARTESIAN_POINT ( 'NONE',  ( 0.1255000000000000282, 1.536931732929928570E-17, -0.6229999999999998872 ) ) ;
#4178 = ORIENTED_EDGE ( 'NONE', *, *, #7079, .T. ) ;
#4179 = CARTESIAN_POINT ( 'NONE',  ( 1.660036532843881085, 1.250860766742396324, 0.1987566293405836071 ) ) ;
#4180 = EDGE_CURVE ( 'NONE', #3239, #1006, #1561, .T. ) ;
#4181 = ADVANCED_FACE ( 'NONE', ( #2832 ), #5914, .T. ) ;
#4182 = EDGE_CURVE ( 'NONE', #4299, #1929, #52, .T. ) ;
#4183 = EDGE_CURVE ( 'NONE', #777, #1018, #2660, .T. ) ;
#4184 = DIRECTION ( 'NONE',  ( 0.000000000000000000, -1.000000000000000000, 0.000000000000000000 ) ) ;
#4185 = CARTESIAN_POINT ( 'NONE',  ( -1.561651944308199313, 0.9741021794092714625, -0.08100000000000007194 ) ) ;
#4186 = MECHANICAL_CONTEXT ( 'NONE', #1369, 'mechanical' ) ;
#4187 = ORIENTED_EDGE ( 'NONE', *, *, #2723, .T. ) ;
#4188 = DIRECTION ( 'NONE',  ( 1.000000000000000000, 0.000000000000000000, 0.000000000000000000 ) ) ;
#4189 = LINE ( 'NONE', #2583, #1515 ) ;
#4190 = EDGE_CURVE ( 'NONE', #3779, #7259, #6738, .T. ) ;
#4191 = LINE ( 'NONE', #4764, #5535 ) ;
#4192 = EDGE_CURVE ( 'NONE', #7906, #5277, #5167, .T. ) ;
#4193 = EDGE_LOOP ( 'NONE', ( #1271, #7804 ) ) ;
#4194 = EDGE_CURVE ( 'NONE', #2343, #7593, #868, .T. ) ;
#4195 = SHAPE_REPRESENTATION ( 'MAS-157, Fastener', ( #416, #4479, #6971 ), #3300 ) ;
#4196 = ORIENTED_EDGE ( 'NONE', *, *, #4183, .F. ) ;
#4197 = ORIENTED_EDGE ( 'NONE', *, *, #3398, .T. ) ;
#4198 = CARTESIAN_POINT ( 'NONE',  ( 0.1210307295689817542, 0.6124999999999999334, -0.03125000000000000000 ) ) ;
#4199 = CARTESIAN_POINT ( 'NONE',  ( 1.416910847748826363, 1.162394599040469156, 0.2206240621652085232 ) ) ;
#4200 = DATE_AND_TIME ( #6131, #5563 ) ;
#4201 = CC_DESIGN_DATE_AND_TIME_ASSIGNMENT ( #914, #7050, ( #418 ) ) ;
#4202 = CARTESIAN_POINT ( 'NONE',  ( 1.537647474970341932, 1.850702997413674389, 0.03199999999999999373 ) ) ;
#4203 = EDGE_CURVE ( 'NONE', #7797, #7184, #5951, .T. ) ;
#4204 = CARTESIAN_POINT ( 'NONE',  ( 6.067840808230170246, 0.2405569712445295161, 5.393636709996481038 ) ) ;
#4205 = LINE ( 'NONE', #3674, #1261 ) ;
#4206 = DIRECTION ( 'NONE',  ( 1.000000000000000000, 0.000000000000000000, 0.000000000000000000 ) ) ;
#4207 = APPLICATION_CONTEXT ( 'configuration controlled 3d designs of mechanical parts and assemblies' ) ;
#4208 = APPROVAL_STATUS ( 'not_yet_approved' ) ;
#4209 = LINE ( 'NONE', #6750, #5068 ) ;
#4210 = ORIENTED_EDGE ( 'NONE', *, *, #8072, .F. ) ;
#4211 = ORIENTED_EDGE ( 'NONE', *, *, #11, .F. ) ;
#4212 = FACE_OUTER_BOUND ( 'NONE', #6656, .T. ) ;
#4213 = DIRECTION ( 'NONE',  ( -1.000000000000000000, 0.000000000000000000, 0.000000000000000000 ) ) ;
#4214 = B_SPLINE_CURVE_WITH_KNOTS ( 'NONE', 3,
 ( #7061, #3942, #6443, #826 ),
 .UNSPECIFIED., .F., .F.,
 ( 4, 4 ),
 ( 1.312212654013605714E-14, 0.001617146350552977566 ),
 .UNSPECIFIED. ) ;
#4215 = ORIENTED_EDGE ( 'NONE', *, *, #7151, .F. ) ;
#4216 = CARTESIAN_POINT ( 'NONE',  ( -4.882388066182508091, 5.670153330992292240, 0.2179999999999999993 ) ) ;
#4217 = DIRECTION ( 'NONE',  ( -0.000000000000000000, 1.000000000000000000, -0.000000000000000000 ) ) ;
#4218 = CARTESIAN_POINT ( 'NONE',  ( -0.02822771919328412663, 0.03615965030273324970, 0.1250000000000000000 ) ) ;
#4219 = ORIENTED_EDGE ( 'NONE', *, *, #4545, .F. ) ;
#4220 = EDGE_LOOP ( 'NONE', ( #7601, #7579 ) ) ;
#4221 = DIRECTION ( 'NONE',  ( 0.000000000000000000, 1.000000000000000000, 0.000000000000000000 ) ) ;
#4222 = AXIS2_PLACEMENT_3D ( 'NONE', #1506, #1456, #853 ) ;
#4223 = CARTESIAN_POINT ( 'NONE',  ( -1.200662090268964421, -0.2165239078499182623, 0.006252944700127002244 ) ) ;
#4224 = CARTESIAN_POINT ( 'NONE',  ( 1.639694973349331120, 1.319210621310791920, 0.2298487237779671677 ) ) ;
#4225 = APPLICATION_PROTOCOL_DEFINITION ( 'international standard', 'config_control_design', 1994, #2361 ) ;
#4226 = VERTEX_POINT ( 'NONE', #1288 ) ;
#4227 = AXIS2_PLACEMENT_3D ( 'NONE', #2828, #5338, #4712 ) ;
#4228 = CARTESIAN_POINT ( 'NONE',  ( 0.2935750530104211387, 0.05119392622207447063, 0.07449999999999999678 ) ) ;
#4229 = DIRECTION ( 'NONE',  ( -0.6568496200222107007, -0.7540216022612862279, 0.000000000000000000 ) ) ;
#4230 = EDGE_CURVE ( 'NONE', #4985, #810, #320, .T. ) ;
#4231 = DIRECTION ( 'NONE',  ( -0.6930146854867019757, -0.5415747525367520243, 0.4758439167568747630 ) ) ;
#4232 = CIRCLE ( 'NONE', #4622, 0.1100000000000000006 ) ;
#4233 = VERTEX_POINT ( 'NONE', #2180 ) ;
#4234 = VERTEX_POINT ( 'NONE', #4559 ) ;
#4235 = ORIENTED_EDGE ( 'NONE', *, *, #7078, .T. ) ;
#4236 = EDGE_LOOP ( 'NONE', ( #38, #5733, #7463, #5379 ) ) ;
#4237 = DIRECTION ( 'NONE',  ( 0.6157549048526804736, -0.7879377495398138809, 0.000000000000000000 ) ) ;
#4238 = PERSON_AND_ORGANIZATION_ROLE ( 'classification_officer' ) ;
#4239 = FACE_OUTER_BOUND ( 'NONE', #7395, .T. ) ;
#4240 = ADVANCED_FACE ( 'NONE', ( #2137 ), #6565, .F. ) ;
#4241 = AXIS2_PLACEMENT_3D ( 'NONE', #1096, #6710, #7325 ) ;
#4242 = ORIENTED_EDGE ( 'NONE', *, *, #1374, .T. ) ;
#4243 = EDGE_CURVE ( 'NONE', #5676, #526, #7648, .T. ) ;
#4244 = ORIENTED_EDGE ( 'NONE', *, *, #7583, .T. ) ;
#4245 = AXIS2_PLACEMENT_3D ( 'NONE', #2350, #3053, #3101 ) ;
#4246 = EDGE_CURVE ( 'NONE', #5062, #668, #819, .T. ) ;
#4247 = CIRCLE ( 'NONE', #3586, 0.1875000000000000278 ) ;
#4248 = ORIENTED_EDGE ( 'NONE', *, *, #1040, .F. ) ;
#4249 = EDGE_CURVE ( 'NONE', #7062, #477, #3325, .T. ) ;
#4250 = CARTESIAN_POINT ( 'NONE',  ( 1.400290408515991292, 1.047875251497336402, -0.1039999999999998703 ) ) ;
#4251 = CARTESIAN_POINT ( 'NONE',  ( 0.000000000000000000, 0.6124999999999999334, 0.03125000000000000000 ) ) ;
#4252 = CARTESIAN_POINT ( 'NONE',  ( 0.04629178820765882107, -0.4636611426331366248, 0.01068174274968844602 ) ) ;
#4253 = CALENDAR_DATE ( 2026, 9, 10 ) ;
#4254 = DIRECTION ( 'NONE',  ( -0.000000000000000000, -0.000000000000000000, -1.000000000000000000 ) ) ;
#4255 = CARTESIAN_POINT ( 'NONE',  ( 1.517690421940173007, 1.264920623133992006, 0.2499999999999999167 ) ) ;
#4256 = CARTESIAN_POINT ( 'NONE',  ( 1.583224725446250369, 1.282100267436459884, 0.2376555858899458973 ) ) ;
#4257 = LOCAL_TIME ( 14, 45, 32.00000000000000000, #5173 ) ;
#4258 = CIRCLE ( 'NONE', #6346, 4.000000000000000888 ) ;
#4259 = DIRECTION ( 'NONE',  ( 1.000000000000000000, 0.000000000000000000, 0.000000000000000000 ) ) ;
#4260 = VECTOR ( 'NONE', #6751, 39.37007874015747433 ) ;
#4261 = TOROIDAL_SURFACE ( 'NONE', #5312, 0.1255000000000000282, 0.06199999999999999956 ) ;
#4262 = EDGE_LOOP ( 'NONE', ( #7012, #4436, #7150, #6965 ) ) ;
#4263 = CARTESIAN_POINT ( 'NONE',  ( -0.1255000000000000282, 0.000000000000000000, -0.5599999999999999423 ) ) ;
#4264 = CARTESIAN_POINT ( 'NONE',  ( 1.288576881684712072, 1.062104608988174492, -0.04610097113422258197 ) ) ;
#4265 = CARTESIAN_POINT ( 'NONE',  ( 1.800320205903116921, 1.030513867073702183, -0.08212881570848259982 ) ) ;
#4266 = ORIENTED_EDGE ( 'NONE', *, *, #729, .F. ) ;
#4267 = ORIENTED_EDGE ( 'NONE', *, *, #2080, .T. ) ;
#4268 = DIRECTION ( 'NONE',  ( 0.6157549048526729241, -0.7879377495398196540, 0.000000000000000000 ) ) ;
#4269 = FACE_OUTER_BOUND ( 'NONE', #4321, .T. ) ;
#4270 = DIRECTION ( 'NONE',  ( 0.000000000000000000, 1.000000000000000000, 0.000000000000000000 ) ) ;
#4271 = AXIS2_PLACEMENT_3D ( 'NONE', #2549, #2710, #6441 ) ;
#4272 = DATE_AND_TIME ( #3615, #2898 ) ;
#4273 = ORIENTED_EDGE ( 'NONE', *, *, #3836, .T. ) ;
#4274 = DIRECTION ( 'NONE',  ( 0.000000000000000000, 1.000000000000000000, 0.000000000000000000 ) ) ;
#4275 = CYLINDRICAL_SURFACE ( 'NONE', #3091, 4.000000000000000888 ) ;
#4276 = VERTEX_POINT ( 'NONE', #7137 ) ;
#4277 = DIRECTION ( 'NONE',  ( 0.000000000000000000, 1.000000000000000000, 0.000000000000000000 ) ) ;
#4278 = AXIS2_PLACEMENT_3D ( 'NONE', #199, #2825, #5909 ) ;
#4279 = ORIENTED_EDGE ( 'NONE', *, *, #7261, .T. ) ;
#4280 = AXIS2_PLACEMENT_3D ( 'NONE', #2740, #4671, #3440 ) ;
#4281 = AXIS2_PLACEMENT_3D ( 'NONE', #2744, #7132, #7052 ) ;
#4282 = DIRECTION ( 'NONE',  ( 0.7879377495398141029, 0.6157549048526802515, 0.000000000000000000 ) ) ;
#4283 = CARTESIAN_POINT ( 'NONE',  ( -1.763630694164995738, 1.150051601412734215, -0.3269762307749163877 ) ) ;
#4284 = PERSON_AND_ORGANIZATION ( #4344, #3069 ) ;
#4285 = DIRECTION ( 'NONE',  ( 1.000000000000000000, 0.000000000000000000, 0.000000000000000000 ) ) ;
#4286 = AXIS2_PLACEMENT_3D ( 'NONE', #1954, #3843, #726 ) ;
#4287 = ADVANCED_FACE ( 'NONE', ( #2705 ), #7712, .T. ) ;
#4288 = CARTESIAN_POINT ( 'NONE',  ( 1.640223930654117312, 1.235377681993896193, -0.4064878104020026583 ) ) ;
#4289 = DIRECTION ( 'NONE',  ( -0.000000000000000000, -0.000000000000000000, -1.000000000000000000 ) ) ;
#4290 = AXIS2_PLACEMENT_3D ( 'NONE', #4829, #7279, #4292 ) ;
#4291 = PERSON_AND_ORGANIZATION_ROLE ( 'creator' ) ;
#4292 = DIRECTION ( 'NONE',  ( -1.000000000000000000, 0.000000000000000000, 0.000000000000000000 ) ) ;
#4293 = AXIS2_PLACEMENT_3D ( 'NONE', #4484, #1489, #6983 ) ;
#4294 = CARTESIAN_POINT ( 'NONE',  ( 1.559972549391304364, 1.821735304801280986, -0.05091778041741192723 ) ) ;
#4295 = EDGE_LOOP ( 'NONE', ( #5034, #6013, #6456, #1855 ) ) ;
#4296 = CARTESIAN_POINT ( 'NONE',  ( 1.621159559802907379, 1.311822379805967387, 0.2374608280823977957 ) ) ;
#4297 = FACE_OUTER_BOUND ( 'NONE', #7637, .T. ) ;
#4298 = ORIENTED_EDGE ( 'NONE', *, *, #5692, .F. ) ;
#4299 = VERTEX_POINT ( 'NONE', #4593 ) ;
#4300 = DIRECTION ( 'NONE',  ( 0.000000000000000000, 1.000000000000000000, 0.000000000000000000 ) ) ;
#4301 = CARTESIAN_POINT ( 'NONE',  ( 1.308306517172985961, 1.069052077891893493, -0.1016069337487079394 ) ) ;
#4302 = PLANE ( 'NONE',  #7414 ) ;
#4303 = VERTEX_POINT ( 'NONE', #3412 ) ;
#4304 = VERTEX_POINT ( 'NONE', #5299 ) ;
#4305 = FACE_OUTER_BOUND ( 'NONE', #193, .T. ) ;
#4306 = LINE ( 'NONE', #8057, #2678 ) ;
#4307 = CARTESIAN_POINT ( 'NONE',  ( 0.1250000000000000278, 0.03125000000000000000, 0.000000000000000000 ) ) ;
#4308 = DATE_AND_TIME ( #8018, #150 ) ;
#4309 = VERTEX_POINT ( 'NONE', #7093 ) ;
#4310 = CARTESIAN_POINT ( 'NONE',  ( 0.1250000000000000000, 0.6250000000000000000, -0.03125000000000000000 ) ) ;
#4311 = PLANE ( 'NONE',  #203 ) ;
#4312 = ORIENTED_EDGE ( 'NONE', *, *, #7635, .T. ) ;
#4313 = DIRECTION ( 'NONE',  ( 0.000000000000000000, 0.000000000000000000, -1.000000000000000000 ) ) ;
#4314 = APPLICATION_CONTEXT ( 'configuration controlled 3d designs of mechanical parts and assemblies' ) ;
#4315 = ORIENTED_EDGE ( 'NONE', *, *, #4636, .F. ) ;
#4316 = DIRECTION ( 'NONE',  ( 1.000000000000000000, 0.000000000000000000, 0.000000000000000000 ) ) ;
#4317 = CARTESIAN_POINT ( 'NONE',  ( -4.521705384338368994, -3.437882612028420048, 0.000000000000000000 ) ) ;
#4318 = COORDINATED_UNIVERSAL_TIME_OFFSET ( 0, 0, .AHEAD. ) ;
#4319 = DIRECTION ( 'NONE',  ( 0.000000000000000000, 0.000000000000000000, -1.000000000000000000 ) ) ;
#4320 = ORIENTED_EDGE ( 'NONE', *, *, #942, .T. ) ;
#4321 = EDGE_LOOP ( 'NONE', ( #922, #4219, #5611, #256 ) ) ;
#4322 = ORIENTED_EDGE ( 'NONE', *, *, #7537, .T. ) ;
#4323 = DIRECTION ( 'NONE',  ( 1.000000000000000000, 0.000000000000000000, 0.000000000000000000 ) ) ;
#4324 = DIRECTION ( 'NONE',  ( 0.000000000000000000, 0.000000000000000000, 1.000000000000000000 ) ) ;
#4325 = CARTESIAN_POINT ( 'NONE',  ( 6.067840808230170246, 0.2405569712445295161, 0.1250000000000004441 ) ) ;
#4326 = APPROVAL_STATUS ( 'not_yet_approved' ) ;
#4327 = PLANE ( 'NONE',  #7558 ) ;
#4328 = CARTESIAN_POINT ( 'NONE',  ( 1.537180804724851413, 1.279018702714873612, 0.2500000000000000555 ) ) ;
#4329 = DIRECTION ( 'NONE',  ( 0.04906492035527430795, -0.9987955914953422498, 0.000000000000000000 ) ) ;
#4330 = ADVANCED_FACE ( 'NONE', ( #7787 ), #4678, .T. ) ;
#4331 = ORIENTED_EDGE ( 'NONE', *, *, #4833, .F. ) ;
#4332 = DIRECTION ( 'NONE',  ( 0.6568496200222107007, 0.7540216022612863389, -0.000000000000000000 ) ) ;
#4333 = CARTESIAN_POINT ( 'NONE',  ( 0.1743677072153199392, -0.4209564106690024676, -0.1250000000000000000 ) ) ;
#4334 = DIRECTION ( 'NONE',  ( -1.000000000000000000, -0.000000000000000000, -0.000000000000000000 ) ) ;
#4335 = ADVANCED_FACE ( 'NONE', ( #4269 ), #2252, .F. ) ;
#4336 = ORIENTED_EDGE ( 'NONE', *, *, #4690, .T. ) ;
#4337 = ADVANCED_FACE ( 'NONE', ( #6070 ), #1358, .T. ) ;
#4338 = ORIENTED_EDGE ( 'NONE', *, *, #2659, .T. ) ;
#4339 = DIRECTION ( 'NONE',  ( -0.6157549048526802515, 0.7879377495398141029, -0.000000000000000000 ) ) ;
#4340 = EDGE_CURVE ( 'NONE', #1116, #305, #2280, .T. ) ;
#4341 = APPROVAL ( #5081, 'UNSPECIFIED' ) ;
#4342 = EDGE_CURVE ( 'NONE', #822, #1921, #3005, .T. ) ;
#4343 = FACE_OUTER_BOUND ( 'NONE', #4707, .T. ) ;
#4344 = PERSON ( 'NAUO-PER7', 'UNSPECIFIED', 'UNSPECIFIED', ('UNSPECIFIED'), ('UNSPECIFIED'), ('UNSPECIFIED') ) ;
#4345 = APPROVAL_PERSON_ORGANIZATION ( #5260, #3691, #3414 ) ;
#4346 = EDGE_CURVE ( 'NONE', #365, #81, #7333, .T. ) ;
#4347 = CARTESIAN_POINT ( 'NONE',  ( 1.667733449989331929, 1.335098490384043712, 0.2216602983319173603 ) ) ;
#4348 = CALENDAR_DATE ( 2026, 9, 10 ) ;
#4349 = EDGE_LOOP ( 'NONE', ( #458, #3811, #5195, #1831 ) ) ;
#4350 = CARTESIAN_POINT ( 'NONE',  ( -0.9142296270274463676, 0.5739542246721701657, -0.1250000000000000000 ) ) ;
#4351 = LINE ( 'NONE', #6848, #467 ) ;
#4352 = DIRECTION ( 'NONE',  ( 0.6157549048509018963, -0.7879377495412036581, 0.000000000000000000 ) ) ;
#4353 = CC_DESIGN_APPROVAL ( #8089, ( #830 ) ) ;
#4354 = LOCAL_TIME ( 14, 45, 32.00000000000000000, #1534 ) ;
#4355 = VERTEX_POINT ( 'NONE', #7944 ) ;
#4356 = AXIS2_PLACEMENT_3D ( 'NONE', #1095, #7364, #1055 ) ;
#4357 = ADVANCED_FACE ( 'NONE', ( #2336, #3526, #6027 ), #6157, .F. ) ;
#4358 = DIRECTION ( 'NONE',  ( -1.000000000000000000, 0.000000000000000000, 0.000000000000000000 ) ) ;
#4359 = DIRECTION ( 'NONE',  ( 1.000000000000000000, 0.000000000000000000, 0.000000000000000000 ) ) ;
#4360 = CYLINDRICAL_SURFACE ( 'NONE', #3720, 0.1249999999999999445 ) ;
#4361 = APPROVAL_PERSON_ORGANIZATION ( #2834, #424, #5301 ) ;
#4362 = COORDINATED_UNIVERSAL_TIME_OFFSET ( 0, 0, .AHEAD. ) ;
#4363 = DIRECTION ( 'NONE',  ( 0.000000000000000000, 0.000000000000000000, 1.000000000000000000 ) ) ;
#4364 = VERTEX_POINT ( 'NONE', #6675 ) ;
#4365 = CIRCLE ( 'NONE', #7755, 0.03200000000000000761 ) ;
#4366 = VERTEX_POINT ( 'NONE', #1063 ) ;
#4367 = CARTESIAN_POINT ( 'NONE',  ( 1.525041352626022473, 0.8560022331433567722, -0.08212881570848259982 ) ) ;
#4368 = CIRCLE ( 'NONE', #1877, 3.939999999999463487 ) ;
#4369 = CARTESIAN_POINT ( 'NONE',  ( 0.02203360116805245725, -0.4639491064115316976, 0.005840653693852291065 ) ) ;
#4370 = PERSON_AND_ORGANIZATION ( #4735, #6190 ) ;
#4371 = CARTESIAN_POINT ( 'NONE',  ( 0.8923633780935225079, 0.7607014108325281798, 0.03200000000000000067 ) ) ;
#4372 = CARTESIAN_POINT ( 'NONE',  ( 1.689090369710469330, 1.679451071328251333, 4.008942324862821895E-14 ) ) ;
#4373 = CARTESIAN_POINT ( 'NONE',  ( 1.743841527944330894, 1.301069857420130038, 0.1733065278142748578 ) ) ;
#4374 = ORIENTED_EDGE ( 'NONE', *, *, #2372, .T. ) ;
#4375 = VECTOR ( 'NONE', #473, 39.37007874015748143 ) ;
#4376 = AXIS2_PLACEMENT_3D ( 'NONE', #1733, #4237, #2463 ) ;
#4377 = EDGE_CURVE ( 'NONE', #7593, #3622, #456, .T. ) ;
#4378 = ORIENTED_EDGE ( 'NONE', *, *, #1537, .F. ) ;
#4379 = CARTESIAN_POINT ( 'NONE',  ( -0.1249999999999999445, -0.03125000000000000000, 0.06250000000000000000 ) ) ;
#4380 = LINE ( 'NONE', #5485, #3227 ) ;
#4381 = AXIS2_PLACEMENT_3D ( 'NONE', #763, #2682, #5764 ) ;
#4382 = LINE ( 'NONE', #1874, #5527 ) ;
#4383 = ORIENTED_EDGE ( 'NONE', *, *, #1668, .F. ) ;
#4384 = DIRECTION ( 'NONE',  ( -1.000000000000000000, 0.000000000000000000, 0.000000000000000000 ) ) ;
#4385 = ORIENTED_EDGE ( 'NONE', *, *, #7980, .T. ) ;
#4386 = ORIENTED_EDGE ( 'NONE', *, *, #7838, .T. ) ;
#4387 = VECTOR ( 'NONE', #1519, 39.37007874015748143 ) ;
#4388 = EDGE_CURVE ( 'NONE', #1004, #4051, #1505, .T. ) ;
#4389 = EDGE_CURVE ( 'NONE', #7259, #3779, #64, .T. ) ;
#4390 = EDGE_CURVE ( 'NONE', #2414, #4493, #1596, .T. ) ;
#4391 = VERTEX_POINT ( 'NONE', #2996 ) ;
#4392 = CARTESIAN_POINT ( 'NONE',  ( 1.738743531207847193, 1.407258481967477604, 0.1849942679939103052 ) ) ;
#4393 = CYLINDRICAL_SURFACE ( 'NONE', #5731, 0.03124999999999985428 ) ;
#4394 = PERSON_AND_ORGANIZATION ( #4735, #6190 ) ;
#4395 = ORIENTED_EDGE ( 'NONE', *, *, #1186, .F. ) ;
#4396 = CARTESIAN_POINT ( 'NONE',  ( 1.414905630928118274, 1.059296705655214499, -0.2064098076014010408 ) ) ;
#4397 = CARTESIAN_POINT ( 'NONE',  ( 0.1210307295689817680, 0.6250000000000000000, -0.03125000000000000000 ) ) ;
#4398 = CLOSED_SHELL ( 'NONE', ( #6747, #6991, #946, #4330, #1180, #7189, #2238, #3794, #7884, #7444, #2831, #3894 ) ) ;
#4399 = AXIS2_PLACEMENT_3D ( 'NONE', #1263, #1225, #3155 ) ;
#4400 = VERTEX_POINT ( 'NONE', #2292 ) ;
#4401 = CARTESIAN_POINT ( 'NONE',  ( 1.452776126472616669, 1.185506347939969674, 0.2257575757582501175 ) ) ;
#4402 = CC_DESIGN_PERSON_AND_ORGANIZATION_ASSIGNMENT ( #7760, #3388, ( #6696 ) ) ;
#4403 = EDGE_CURVE ( 'NONE', #4688, #5571, #3347, .T. ) ;
#4404 = ADVANCED_FACE ( 'NONE', ( #2217 ), #5698, .T. ) ;
#4405 = ORIENTED_EDGE ( 'NONE', *, *, #236, .T. ) ;
#4406 = CIRCLE ( 'NONE', #7273, 0.1250000000000000000 ) ;
#4407 = CARTESIAN_POINT ( 'NONE',  ( 1.302790242782180918, 1.667167568704493341, -0.1039999999999998703 ) ) ;
#4408 =( NAMED_UNIT ( * ) SI_UNIT ( $, .STERADIAN. ) SOLID_ANGLE_UNIT ( ) );
#4409 = DIRECTION ( 'NONE',  ( -1.000000000000000000, 0.000000000000000000, 0.000000000000000000 ) ) ;
#4410 = CARTESIAN_POINT ( 'NONE',  ( -0.1255000000000000282, 0.000000000000000000, -0.6849999999999999423 ) ) ;
#4411 = AXIS2_PLACEMENT_3D ( 'NONE', #1963, #2493, #740 ) ;
#4412 = ORIENTED_EDGE ( 'NONE', *, *, #6033, .F. ) ;
#4413 = AXIS2_PLACEMENT_3D ( 'NONE', #7539, #2577, #3313 ) ;
#4414 = AXIS2_PLACEMENT_3D ( 'NONE', #6933, #706, #4514 ) ;
#4415 = ORIENTED_EDGE ( 'NONE', *, *, #7399, .F. ) ;
#4416 = CARTESIAN_POINT ( 'NONE',  ( 1.603331916026614845, 1.035214104258893153, -0.1039999999999998564 ) ) ;
#4417 = CARTESIAN_POINT ( 'NONE',  ( 1.640223930641419914, 1.235377681954054285, -0.08212881570848259982 ) ) ;
#4418 = PERSON_AND_ORGANIZATION_ROLE ( 'creator' ) ;
#4419 = DIRECTION ( 'NONE',  ( 0.2815666759589948720, -0.9595416650617117904, 0.000000000000000000 ) ) ;
#4420 = CARTESIAN_POINT ( 'NONE',  ( 1.566356832197602467, 1.820341369176796009, 2.344234228102034760E-14 ) ) ;
#4421 = ORIENTED_EDGE ( 'NONE', *, *, #1440, .T. ) ;
#4422 = AXIS2_PLACEMENT_3D ( 'NONE', #5688, #5767, #6997 ) ;
#4423 = TOROIDAL_SURFACE ( 'NONE', #1655, 0.09374999999999998612, 0.03125000000000000000 ) ;
#4424 = AXIS2_PLACEMENT_3D ( 'NONE', #4002, #3568, #453 ) ;
#4425 = AXIS2_PLACEMENT_3D ( 'NONE', #3122, #5621, #1842 ) ;
#4426 = EDGE_LOOP ( 'NONE', ( #5542, #7573 ) ) ;
#4427 = LINE ( 'NONE', #3184, #1881 ) ;
#4428 = CARTESIAN_POINT ( 'NONE',  ( -0.09999999999999997780, -0.03125000000000000000, 0.7124999999999989120 ) ) ;
#4429 = CYLINDRICAL_SURFACE ( 'NONE', #2775, 0.03199999999999997985 ) ;
#4430 = ORIENTED_EDGE ( 'NONE', *, *, #2621, .T. ) ;
#4431 = PLANE ( 'NONE',  #303 ) ;
#4432 = ORIENTED_EDGE ( 'NONE', *, *, #7047, .T. ) ;
#4433 = CARTESIAN_POINT ( 'NONE',  ( 0.000000000000000000, -0.03125000000000000000, 0.6646281645421511231 ) ) ;
#4434 = DIRECTION ( 'NONE',  ( 0.000000000000000000, 0.000000000000000000, 1.000000000000000000 ) ) ;
#4435 = APPROVAL_STATUS ( 'not_yet_approved' ) ;
#4436 = ORIENTED_EDGE ( 'NONE', *, *, #4733, .F. ) ;
#4437 = CARTESIAN_POINT ( 'NONE',  ( 1.258671604940865274, -0.02501003737716508274, 0.1850000000000003586 ) ) ;
#4438 = DIRECTION ( 'NONE',  ( -0.6157549048526803626, 0.7879377495398141029, -0.000000000000000000 ) ) ;
#4439 = LINE ( 'NONE', #1272, #7877 ) ;
#4440 = EDGE_CURVE ( 'NONE', #1006, #2215, #5829, .T. ) ;
#4441 = DIRECTION ( 'NONE',  ( -0.000000000000000000, -0.000000000000000000, -1.000000000000000000 ) ) ;
#4442 = EDGE_CURVE ( 'NONE', #7370, #1943, #5341, .T. ) ;
#4443 = LINE ( 'NONE', #3282, #8027 ) ;
#4444 = EDGE_CURVE ( 'NONE', #2638, #3518, #992, .T. ) ;
#4445 = CYLINDRICAL_SURFACE ( 'NONE', #2301, 0.1875000000000000278 ) ;
#4446 = ADVANCED_FACE ( 'NONE', ( #655 ), #8016, .F. ) ;
#4447 = ADVANCED_FACE ( 'NONE', ( #76 ), #6961, .F. ) ;
#4448 = ORIENTED_EDGE ( 'NONE', *, *, #6830, .F. ) ;
#4449 = CC_DESIGN_PERSON_AND_ORGANIZATION_ASSIGNMENT ( #1384, #1843, ( #4603 ) ) ;
#4450 = EDGE_CURVE ( 'NONE', #526, #1756, #4306, .T. ) ;
#4451 =( NAMED_UNIT ( * ) PLANE_ANGLE_UNIT ( ) SI_UNIT ( $, .RADIAN. ) );
#4452 = CARTESIAN_POINT ( 'NONE',  ( 1.949881085063987829, 1.188004538119556086, -0.1039999999999998703 ) ) ;
#4453 = COORDINATED_UNIVERSAL_TIME_OFFSET ( 0, 0, .AHEAD. ) ;
#4454 = DIRECTION ( 'NONE',  ( 0.000000000000000000, 0.000000000000000000, 1.000000000000000000 ) ) ;
#4455 = CARTESIAN_POINT ( 'NONE',  ( -0.04782642554762442377, -0.07812500000000000000, 0.07449999999999999678 ) ) ;
#4456 = ORIENTED_EDGE ( 'NONE', *, *, #3081, .F. ) ;
#4457 = CARTESIAN_POINT ( 'NONE',  ( 0.000000000000000000, 1.050000000000000044, -0.2112499999999999933 ) ) ;
#4458 = ORIENTED_EDGE ( 'NONE', *, *, #330, .F. ) ;
#4459 = CARTESIAN_POINT ( 'NONE',  ( 1.697905879539435725, 1.363584050841088358, 0.2176101576819327310 ) ) ;
#4460 = CARTESIAN_POINT ( 'NONE',  ( 0.000000000000000000, 0.03125000000000000000, -0.1799999999999999933 ) ) ;
#4461 = CARTESIAN_POINT ( 'NONE',  ( 1.778571697411903907, 1.436640564646076035, 0.1446028122283900819 ) ) ;
#4462 = ORIENTED_EDGE ( 'NONE', *, *, #373, .F. ) ;
#4463 = CARTESIAN_POINT ( 'NONE',  ( 2.778417425565558062E-17, 1.112500000000000044, -0.2112499999999999933 ) ) ;
#4464 = LINE ( 'NONE', #1841, #5962 ) ;
#4465 = DIRECTION ( 'NONE',  ( -0.000000000000000000, 0.000000000000000000, 1.000000000000000000 ) ) ;
#4466 = PERSON_AND_ORGANIZATION ( #4735, #6190 ) ;
#4467 = EDGE_LOOP ( 'NONE', ( #965, #1163, #865, #5161, #6406, #2367, #4385, #6678 ) ) ;
#4468 = CARTESIAN_POINT ( 'NONE',  ( -0.1255000000000000282, 1.916572240665608148E-17, 0.000000000000000000 ) ) ;
#4469 = CYLINDRICAL_SURFACE ( 'NONE', #6885, 9.004497838701041701 ) ;
#4470 = DIRECTION ( 'NONE',  ( 0.000000000000000000, 0.000000000000000000, 1.000000000000000000 ) ) ;
#4471 = DIRECTION ( 'NONE',  ( 6.975840231036812635E-15, -1.000000000000000000, -2.013666839457971600E-30 ) ) ;
#4472 = COORDINATED_UNIVERSAL_TIME_OFFSET ( 0, 0, .AHEAD. ) ;
#4473 = DIRECTION ( 'NONE',  ( 0.000000000000000000, 0.000000000000000000, -1.000000000000000000 ) ) ;
#4474 = DIRECTION ( 'NONE',  ( -0.000000000000000000, -0.000000000000000000, -1.000000000000000000 ) ) ;
#4475 = VECTOR ( 'NONE', #54, 39.37007874015748143 ) ;
#4476 = ORIENTED_EDGE ( 'NONE', *, *, #1216, .F. ) ;
#4477 = CARTESIAN_POINT ( 'NONE',  ( 0.9207653111462810180, 0.7459592875503607834, 0.03199999999999999373 ) ) ;
#4478 = AXIS2_PLACEMENT_3D ( 'NONE', #7099, #5612, #3108 ) ;
#4479 = AXIS2_PLACEMENT_3D ( 'NONE', #5226, #883, #2101 ) ;
#4480 = PRODUCT_DEFINITION_FORMATION_WITH_SPECIFIED_SOURCE ( 'ANY', '', #2972, .NOT_KNOWN. ) ;
#4481 = DIRECTION ( 'NONE',  ( 0.000000000000000000, 0.000000000000000000, 1.000000000000000000 ) ) ;
#4482 = ADVANCED_FACE ( 'NONE', ( #1339 ), #7538, .F. ) ;
#4483 = EDGE_CURVE ( 'NONE', #846, #7642, #2165, .T. ) ;
#4484 = CARTESIAN_POINT ( 'NONE',  ( 0.000000000000000000, 1.112500000000000044, 0.000000000000000000 ) ) ;
#4485 = APPROVAL_ROLE ( '' ) ;
#4486 = FACE_OUTER_BOUND ( 'NONE', #6067, .T. ) ;
#4487 = CARTESIAN_POINT ( 'NONE',  ( 0.000000000000000000, 0.000000000000000000, -0.6537499999999999423 ) ) ;
#4488 = AXIS2_PLACEMENT_3D ( 'NONE', #6076, #1114, #1848 ) ;
#4489 = APPROVAL ( #666, 'UNKNOWN' ) ;
#4490 = ADVANCED_FACE ( 'NONE', ( #1806 ), #4962, .T. ) ;
#4491 = ADVANCED_FACE ( 'NONE', ( #4920, #4343 ), #3776, .T. ) ;
#4492 = CIRCLE ( 'NONE', #2792, 0.03125000000000000694 ) ;
#4493 = VERTEX_POINT ( 'NONE', #2576 ) ;
#4494 = DIRECTION ( 'NONE',  ( 0.7879377495398137699, 0.6157549048526805846, 0.000000000000000000 ) ) ;
#4495 = ORIENTED_EDGE ( 'NONE', *, *, #3187, .F. ) ;
#4496 = DIRECTION ( 'NONE',  ( -0.000000000000000000, 1.000000000000000000, -0.000000000000000000 ) ) ;
#4497 = DIRECTION ( 'NONE',  ( -1.000000000000000000, 0.000000000000000000, 0.000000000000000000 ) ) ;
#4498 = CYLINDRICAL_SURFACE ( 'NONE', #6446, 0.4060000000000000830 ) ;
#4499 = CIRCLE ( 'NONE', #973, 0.03200000000000002148 ) ;
#4500 = CARTESIAN_POINT ( 'NONE',  ( -0.09999999999999997780, -0.03125000000000000000, 0.8125000000000000000 ) ) ;
#4501 = VECTOR ( 'NONE', #2270, 39.37007874015748143 ) ;
#4502 = AXIS2_PLACEMENT_3D ( 'NONE', #229, #1331, #7568 ) ;
#4503 = ORIENTED_EDGE ( 'NONE', *, *, #5053, .F. ) ;
#4504 = CARTESIAN_POINT ( 'NONE',  ( 1.487026048750669238, 1.851755883273100922, 0.02040206030734219994 ) ) ;
#4505 = CARTESIAN_POINT ( 'NONE',  ( 1.895798626963228317, 1.435103323869673764, -0.08212881570848257207 ) ) ;
#4506 = PERSON_AND_ORGANIZATION_ROLE ( 'design_supplier' ) ;
#4507 = ORIENTED_EDGE ( 'NONE', *, *, #7489, .T. ) ;
#4508 = FACE_OUTER_BOUND ( 'NONE', #4631, .T. ) ;
#4509 = CARTESIAN_POINT ( 'NONE',  ( 2.030680894239651479, 1.210535352034035839, -0.08212881570848259982 ) ) ;
#4510 = ORIENTED_EDGE ( 'NONE', *, *, #3138, .F. ) ;
#4511 = DIRECTION ( 'NONE',  ( -0.000000000000000000, 0.000000000000000000, -1.000000000000000000 ) ) ;
#4512 = VERTEX_POINT ( 'NONE', #14 ) ;
#4513 = AXIS2_PLACEMENT_3D ( 'NONE', #7961, #6745, #5555 ) ;
#4514 = DIRECTION ( 'NONE',  ( -1.000000000000000000, 0.000000000000000000, 0.000000000000000000 ) ) ;
#4515 = DATE_AND_TIME ( #6255, #6838 ) ;
#4516 = CARTESIAN_POINT ( 'NONE',  ( 1.335403689192364851, 0.9717850835686417943, -0.1039999999999998703 ) ) ;
#4517 = AXIS2_PLACEMENT_3D ( 'NONE', #7327, #2896, #6670 ) ;
#4518 = CARTESIAN_POINT ( 'NONE',  ( 0.000000000000000000, 0.000000000000000000, 0.1250000000000000000 ) ) ;
#4519 = CARTESIAN_POINT ( 'NONE',  ( 1.693285456672191325, 1.338775588042468767, 0.1841458301845965428 ) ) ;
#4520 = CIRCLE ( 'NONE', #460, 0.1100000000000000006 ) ;
#4521 = ORIENTED_EDGE ( 'NONE', *, *, #5442, .F. ) ;
#4522 = CARTESIAN_POINT ( 'NONE',  ( 0.1875000000000000278, 2.296212748401287726E-17, 0.1250000000000000000 ) ) ;
#4523 = ORIENTED_EDGE ( 'NONE', *, *, #1935, .F. ) ;
#4524 = LINE ( 'NONE', #7026, #7298 ) ;
#4525 = SECURITY_CLASSIFICATION_LEVEL ( 'unclassified' ) ;
#4526 = FACE_OUTER_BOUND ( 'NONE', #1412, .T. ) ;
#4527 = CARTESIAN_POINT ( 'NONE',  ( 0.000000000000000000, 0.000000000000000000, 0.06300000000000000044 ) ) ;
#4528 = AXIS2_PLACEMENT_3D ( 'NONE', #2798, #6000, #371 ) ;
#4529 = ORIENTED_EDGE ( 'NONE', *, *, #7536, .F. ) ;
#4530 = ORIENTED_EDGE ( 'NONE', *, *, #2659, .F. ) ;
#4531 = EDGE_LOOP ( 'NONE', ( #3212, #4530, #2802, #5730 ) ) ;
#4532 = EDGE_CURVE ( 'NONE', #3239, #4688, #3611, .T. ) ;
#4533 = EDGE_CURVE ( 'NONE', #4660, #822, #696, .T. ) ;
#4534 = AXIS2_PLACEMENT_3D ( 'NONE', #1514, #5373, #2246 ) ;
#4535 = ORIENTED_EDGE ( 'NONE', *, *, #1978, .F. ) ;
#4536 = EDGE_CURVE ( 'NONE', #5921, #4769, #3693, .T. ) ;
#4537 = VERTEX_POINT ( 'NONE', #3196 ) ;
#4538 = CARTESIAN_POINT ( 'NONE',  ( 0.1000000000000000472, 0.03125000000000000000, 0.8125000000000000000 ) ) ;
#4539 = ORIENTED_EDGE ( 'NONE', *, *, #4483, .F. ) ;
#4541 = CARTESIAN_POINT ( 'NONE',  ( 1.634230631622952457, 1.327686990689322277, 0.2415108169663792437 ) ) ;
#4540 = VECTOR ( 'NONE', #3770, 39.37007874015748143 ) ;
#4542 = CARTESIAN_POINT ( 'NONE',  ( 1.402435059179732990, 1.065697847451554825, -0.1946357965901184539 ) ) ;
#4543 = CIRCLE ( 'NONE', #3107, 0.1875000000000000278 ) ;
#4544 = PRODUCT_RELATED_PRODUCT_CATEGORY ( 'detail', '', ( #3286 ) ) ;
#4545 = EDGE_CURVE ( 'NONE', #777, #1501, #4464, .T. ) ;
#4546 = LINE ( 'NONE', #5283, #7362 ) ;
#4547 = LINE ( 'NONE', #149, #4888 ) ;
#4548 = AXIS2_PLACEMENT_3D ( 'NONE', #1910, #642, #1249 ) ;
#4549 = CIRCLE ( 'NONE', #2057, 7.490657474112464520 ) ;
#4550 = FACE_OUTER_BOUND ( 'NONE', #5012, .T. ) ;
#4551 = CALENDAR_DATE ( 2026, 9, 10 ) ;
#4552 = ORIENTED_EDGE ( 'NONE', *, *, #1586, .F. ) ;
#4553 = DIRECTION ( 'NONE',  ( -0.000000000000000000, 0.000000000000000000, 1.000000000000000000 ) ) ;
#4554 = AXIS2_PLACEMENT_3D ( 'NONE', #701, #2127, #1344 ) ;
#4555 = AXIS2_PLACEMENT_3D ( 'NONE', #2919, #5316, #1610 ) ;
#4556 = DIRECTION ( 'NONE',  ( -1.224646799147352961E-16, 0.000000000000000000, -1.000000000000000000 ) ) ;
#4557 = ORIENTED_EDGE ( 'NONE', *, *, #469, .F. ) ;
#4558 = FACE_OUTER_BOUND ( 'NONE', #7096, .T. ) ;
#4559 = CARTESIAN_POINT ( 'NONE',  ( 0.000000000000000000, 0.03125000000000000000, 0.2731068805941697653 ) ) ;
#4560 = DIRECTION ( 'NONE',  ( -0.000000000000000000, -0.000000000000000000, 1.000000000000000000 ) ) ;
#4561 = PERSON_AND_ORGANIZATION ( #4735, #6190 ) ;
#4562 = FACE_OUTER_BOUND ( 'NONE', #2312, .T. ) ;
#4563 = DIRECTION ( 'NONE',  ( -0.8680936205257657745, 0.4964005096718455690, -1.084872589120758850E-15 ) ) ;
#4564 = DIRECTION ( 'NONE',  ( 0.000000000000000000, 0.000000000000000000, 1.000000000000000000 ) ) ;
#4565 = DIRECTION ( 'NONE',  ( 0.000000000000000000, 0.000000000000000000, 1.000000000000000000 ) ) ;
#4566 = PERSON_AND_ORGANIZATION_ROLE ( 'design_owner' ) ;
#4567 = FACE_OUTER_BOUND ( 'NONE', #6450, .T. ) ;
#4568 = DIRECTION ( 'NONE',  ( -0.000000000000000000, 0.000000000000000000, -1.000000000000000000 ) ) ;
#4569 = VERTEX_POINT ( 'NONE', #565 ) ;
#4570 = VERTEX_POINT ( 'NONE', #7576 ) ;
#4571 = ORIENTED_EDGE ( 'NONE', *, *, #7986, .T. ) ;
#4572 = VERTEX_POINT ( 'NONE', #614 ) ;
#4573 = CARTESIAN_POINT ( 'NONE',  ( 0.1255000000000000282, 0.000000000000000000, 0.000000000000000000 ) ) ;
#4574 = ORIENTED_EDGE ( 'NONE', *, *, #5539, .F. ) ;
#4575 = CARTESIAN_POINT ( 'NONE',  ( 1.697466594803655804, 1.379849898015399035, 0.2127906551866314833 ) ) ;
#4576 = PLANE ( 'NONE',  #4422 ) ;
#4577 = CARTESIAN_POINT ( 'NONE',  ( 2.054765106439577771, 0.7510910599158125978, 0.1250000000000000000 ) ) ;
#4578 = VERTEX_POINT ( 'NONE', #6352 ) ;
#4579 = DIRECTION ( 'NONE',  ( -1.000000000000000000, 0.000000000000000000, 0.000000000000000000 ) ) ;
#4580 = ORIENTED_EDGE ( 'NONE', *, *, #7300, .T. ) ;
#4581 = CARTESIAN_POINT ( 'NONE',  ( 1.528725049572218664, 1.845702208139184064, 0.03396726950201266887 ) ) ;
#4582 = DIRECTION ( 'NONE',  ( 0.000000000000000000, 0.000000000000000000, -1.000000000000000000 ) ) ;
#4583 = PERSON_AND_ORGANIZATION ( #4735, #6190 ) ;
#4584 = ADVANCED_FACE ( 'NONE', ( #6194 ), #5078, .T. ) ;
#4585 = DIRECTION ( 'NONE',  ( 0.000000000000000000, -1.000000000000000000, 0.000000000000000000 ) ) ;
#4586 = DIRECTION ( 'NONE',  ( 1.000000000000000000, 0.000000000000000000, 0.000000000000000000 ) ) ;
#4587 = DIRECTION ( 'NONE',  ( -0.000000000000000000, -0.000000000000000000, -1.000000000000000000 ) ) ;
#4588 = VERTEX_POINT ( 'NONE', #7609 ) ;
#4589 = EDGE_CURVE ( 'NONE', #4572, #5716, #6228, .T. ) ;
#4590 = CARTESIAN_POINT ( 'NONE',  ( -0.6495791112554195612, -0.6379566159512914947, 0.2179999999999999993 ) ) ;
#4591 = APPROVAL ( #7446, 'UNSPECIFIED' ) ;
#4592 = ADVANCED_FACE ( 'NONE', ( #7129 ), #1979, .T. ) ;
#4593 = CARTESIAN_POINT ( 'NONE',  ( -0.1875000000000000278, 2.296212748401287726E-17, -0.6229999999999998872 ) ) ;
#4594 = CARTESIAN_POINT ( 'NONE',  ( 1.537935346170436812, 1.852967428140057216, 0.000000000000000000 ) ) ;
#4595 = PERSON_AND_ORGANIZATION ( #4735, #6190 ) ;
#4596 = ORIENTED_EDGE ( 'NONE', *, *, #482, .T. ) ;
#4597 = DIRECTION ( 'NONE',  ( -0.000000000000000000, 0.000000000000000000, -1.000000000000000000 ) ) ;
#4598 = CARTESIAN_POINT ( 'NONE',  ( 1.761384412048883741, 1.314317347873839692, 0.1623010253713057793 ) ) ;
#4599 = EDGE_LOOP ( 'NONE', ( #50, #2281 ) ) ;
#4600 =( NAMED_UNIT ( * ) SI_UNIT ( $, .STERADIAN. ) SOLID_ANGLE_UNIT ( ) );
#4601 = CYLINDRICAL_SURFACE ( 'NONE', #3978, 6.870657474112407570 ) ;
#4602 = CARTESIAN_POINT ( 'NONE',  ( -1.723766588794375387, 1.115324847714046497, -0.08100000000000007194 ) ) ;
#4603 = PRODUCT_DEFINITION_FORMATION_WITH_SPECIFIED_SOURCE ( 'ANY', '', #7731, .NOT_KNOWN. ) ;
#4604 = CONTEXT_DEPENDENT_SHAPE_REPRESENTATION ( #5995, #278 ) ;
#4605 = LINE ( 'NONE', #6074, #6905 ) ;
#4606 = DIRECTION ( 'NONE',  ( 1.224646799147352961E-16, 0.000000000000000000, -1.000000000000000000 ) ) ;
#4607 = ORIENTED_EDGE ( 'NONE', *, *, #6457, .F. ) ;
#4608 = EDGE_LOOP ( 'NONE', ( #4674, #5554, #2730, #5501 ) ) ;
#4609 = CIRCLE ( 'NONE', #2256, 0.1100000000000000006 ) ;
#4610 = ORIENTED_EDGE ( 'NONE', *, *, #5602, .T. ) ;
#4611 = PRODUCT_DEFINITION_FORMATION_WITH_SPECIFIED_SOURCE ( 'ANY', '', #2761, .NOT_KNOWN. ) ;
#4612 = VERTEX_POINT ( 'NONE', #4708 ) ;
#4613 = ORIENTED_EDGE ( 'NONE', *, *, #1941, .T. ) ;
#4614 = DIRECTION ( 'NONE',  ( 0.7013568910933712930, 0.4952151427499992820, -0.5126992039265700907 ) ) ;
#4615 = VERTEX_POINT ( 'NONE', #3478 ) ;
#4616 = CIRCLE ( 'NONE', #6321, 8.573908398499121120 ) ;
#4617 = CARTESIAN_POINT ( 'NONE',  ( -1.615754213267370121, 0.7559880647407505316, 0.1720737575213688586 ) ) ;
#4618 = CARTESIAN_POINT ( 'NONE',  ( 2.204364238465235822E-17, 0.03125000000000000000, 0.1799999999999999933 ) ) ;
#4619 = CARTESIAN_POINT ( 'NONE',  ( -0.1210307295689817542, 0.6124999999999999334, -0.03125000000000000000 ) ) ;
#4620 = ORIENTED_EDGE ( 'NONE', *, *, #7234, .T. ) ;
#4621 = CARTESIAN_POINT ( 'NONE',  ( -0.1249999999999999445, -0.03125000000000000000, 0.000000000000000000 ) ) ;
#4622 = AXIS2_PLACEMENT_3D ( 'NONE', #2289, #492, #5452 ) ;
#4623 = VERTEX_POINT ( 'NONE', #1671 ) ;
#4624 = CARTESIAN_POINT ( 'NONE',  ( 1.788409570110391256, 1.426923381411736358, 0.1429701060512907629 ) ) ;
#4625 = DIRECTION ( 'NONE',  ( 0.7879377495385916363, 0.6157549048542446668, 0.000000000000000000 ) ) ;
#4626 = CALENDAR_DATE ( 2026, 9, 10 ) ;
#4627 = CARTESIAN_POINT ( 'NONE',  ( -1.410683006424825692, 0.8425888524880515984, 0.2499905547878000789 ) ) ;
#4628 = CIRCLE ( 'NONE', #1097, 0.06199999999999999956 ) ;
#4629 = FACE_OUTER_BOUND ( 'NONE', #7441, .T. ) ;
#4630 = FACE_OUTER_BOUND ( 'NONE', #2402, .T. ) ;
#4631 = EDGE_LOOP ( 'NONE', ( #1820, #4279, #1494, #2158 ) ) ;
#4632 = ORIENTED_EDGE ( 'NONE', *, *, #1029, .F. ) ;
#4633 = DIRECTION ( 'NONE',  ( 0.2791259188691606608, 0.9602545086670756236, 0.000000000000000000 ) ) ;
#4634 = AXIS2_PLACEMENT_3D ( 'NONE', #2316, #640, #7445 ) ;
#4635 = ADVANCED_FACE ( 'NONE', ( #4175 ), #7290, .F. ) ;
#4636 = EDGE_CURVE ( 'NONE', #4309, #2414, #1677, .T. ) ;
#4637 = AXIS2_PLACEMENT_3D ( 'NONE', #3864, #46, #7059 ) ;
#4638 = CARTESIAN_POINT ( 'NONE',  ( 0.000000000000000000, 0.000000000000000000, 0.000000000000000000 ) ) ;
#4639 = CARTESIAN_POINT ( 'NONE',  ( 6.190219624525621356, 0.4584813330253886265, -0.1849999999999999978 ) ) ;
#4640 = COORDINATED_UNIVERSAL_TIME_OFFSET ( 0, 0, .AHEAD. ) ;
#4641 = ORIENTED_EDGE ( 'NONE', *, *, #7394, .T. ) ;
#4642 = CC_DESIGN_PERSON_AND_ORGANIZATION_ASSIGNMENT ( #540, #3010, ( #1357 ) ) ;
#4643 = EDGE_LOOP ( 'NONE', ( #3696, #692 ) ) ;
#4644 = CARTESIAN_POINT ( 'NONE',  ( 0.3037060500451564393, -0.3811688768094762536, 0.2500000000000003331 ) ) ;
#4645 = ORGANIZATION ( 'NAUO-ORG3', 'UNSPECIFIED', 'UNSPECIFIED' ) ;
#4646 = ADVANCED_FACE ( 'NONE', ( #7206 ), #5405, .T. ) ;
#4647 = CIRCLE ( 'NONE', #4513, 0.03124999999999997571 ) ;
#4648 = CARTESIAN_POINT ( 'NONE',  ( 1.258616368121236118, -0.02482036781376564805, -0.1250000000000000000 ) ) ;
#4649 = ADVANCED_FACE ( 'NONE', ( #1628, #944 ), #4834, .T. ) ;
#4650 = EDGE_LOOP ( 'NONE', ( #2223, #1066, #3290, #2999 ) ) ;
#4651 = ORIENTED_EDGE ( 'NONE', *, *, #2084, .F. ) ;
#4652 = VECTOR ( 'NONE', #3012, 39.37007874015748143 ) ;
#4653 =( NAMED_UNIT ( * ) PLANE_ANGLE_UNIT ( ) SI_UNIT ( $, .RADIAN. ) );
#4654 = DIRECTION ( 'NONE',  ( 1.224646799147353207E-16, 1.000000000000000000, -0.000000000000000000 ) ) ;
#4655 = CARTESIAN_POINT ( 'NONE',  ( -1.543211452806561912, 0.6927940070358482583, -0.1250000000000000000 ) ) ;
#4656 = DATE_TIME_ROLE ( 'classification_date' ) ;
#4657 = CARTESIAN_POINT ( 'NONE',  ( 1.858819419417630847, 1.479091072822390718, -0.004310541304807894401 ) ) ;
#4658 = CIRCLE ( 'NONE', #6621, 0.3099999999999745737 ) ;
#4659 = AXIS2_PLACEMENT_3D ( 'NONE', #5371, #7851, #440 ) ;
#4660 = VERTEX_POINT ( 'NONE', #1057 ) ;
#4661 = EDGE_LOOP ( 'NONE', ( #1779, #6477, #3672, #6732 ) ) ;
#4662 = DIRECTION ( 'NONE',  ( 0.000000000000000000, 0.000000000000000000, 1.000000000000000000 ) ) ;
#4663 = ORIENTED_EDGE ( 'NONE', *, *, #989, .F. ) ;
#4664 = DIRECTION ( 'NONE',  ( -0.000000000000000000, -0.000000000000000000, -1.000000000000000000 ) ) ;
#4665 = CARTESIAN_POINT ( 'NONE',  ( -1.542052804988285786, 0.6917846760340663481, 0.2499905547878000789 ) ) ;
#4666 = LINE ( 'NONE', #7042, #2376 ) ;
#4667 = CYLINDRICAL_SURFACE ( 'NONE', #970, 0.1799999999999999933 ) ;
#4668 = VECTOR ( 'NONE', #4587, 39.37007874015748143 ) ;
#4669 = AXIS2_PLACEMENT_3D ( 'NONE', #363, #4176, #2778 ) ;
#4670 = CARTESIAN_POINT ( 'NONE',  ( 1.807005629368180655, 1.428622671733608129, 0.1122175490488539484 ) ) ;
#4671 = DIRECTION ( 'NONE',  ( 0.000000000000000000, 0.000000000000000000, -1.000000000000000000 ) ) ;
#4672 = PLANE ( 'NONE',  #6117 ) ;
#4673 = DIRECTION ( 'NONE',  ( 0.000000000000000000, 0.000000000000000000, 1.000000000000000000 ) ) ;
#4674 = ORIENTED_EDGE ( 'NONE', *, *, #7875, .F. ) ;
#4675 = AXIS2_PLACEMENT_3D ( 'NONE', #4665, #1017, #3516 ) ;
#4676 = CARTESIAN_POINT ( 'NONE',  ( 1.399572429561498188, 1.060126801036724631, -0.1797357540389955821 ) ) ;
#4677 = CIRCLE ( 'NONE', #1931, 0.03200000000000005618 ) ;
#4678 = PLANE ( 'NONE',  #5165 ) ;
#4679 = AXIS2_PLACEMENT_3D ( 'NONE', #4963, #7334, #2997 ) ;
#4680 = CARTESIAN_POINT ( 'NONE',  ( 1.536310283592701609, 1.851420836617818422, -0.007424632097850032350 ) ) ;
#4681 = DATE_TIME_ROLE ( 'creation_date' ) ;
#4682 = EDGE_LOOP ( 'NONE', ( #7473, #501, #2192, #6497 ) ) ;
#4683 = DIRECTION ( 'NONE',  ( -0.7879377495398141029, -0.6157549048526802515, 0.000000000000000000 ) ) ;
#4684 = EDGE_CURVE ( 'NONE', #2070, #5954, #3604, .T. ) ;
#4685 = EDGE_CURVE ( 'NONE', #2075, #6542, #2864, .T. ) ;
#4686 = CARTESIAN_POINT ( 'NONE',  ( 1.437142212823544263, 1.212327995211806453, 0.2500000000000000000 ) ) ;
#4687 = ADVANCED_FACE ( 'NONE', ( #6594 ), #362, .F. ) ;
#4688 = VERTEX_POINT ( 'NONE', #321 ) ;
#4689 = ORIENTED_EDGE ( 'NONE', *, *, #2321, .T. ) ;
#4690 = EDGE_CURVE ( 'NONE', #6271, #6313, #7528, .T. ) ;
#4691 = ORIENTED_EDGE ( 'NONE', *, *, #985, .F. ) ;
#4692 = FACE_OUTER_BOUND ( 'NONE', #1378, .T. ) ;
#4693 = CARTESIAN_POINT ( 'NONE',  ( 1.850068364776406682, 1.494658567734585608, 0.000000000000000000 ) ) ;
#4694 = ADVANCED_FACE ( 'NONE', ( #2943 ), #7784, .T. ) ;
#4695 = EDGE_CURVE ( 'NONE', #6698, #4355, #6635, .T. ) ;
#4696 = ADVANCED_FACE ( 'NONE', ( #1709 ), #6488, .T. ) ;
#4697 = ORIENTED_EDGE ( 'NONE', *, *, #5738, .T. ) ;
#4698 = APPROVAL ( #7519, 'UNSPECIFIED' ) ;
#4699 = ADVANCED_FACE ( 'NONE', ( #6022 ), #4261, .T. ) ;
#4700 = ORIENTED_EDGE ( 'NONE', *, *, #7489, .F. ) ;
#4701 = CARTESIAN_POINT ( 'NONE',  ( 2.387087291339119677, -6.013863021948615106, 0.1250000000000000000 ) ) ;
#4702 = CARTESIAN_POINT ( 'NONE',  ( 15385.63906443092310, -19685.02381974099626, -0.2249973011472257700 ) ) ;
#4703 = DIRECTION ( 'NONE',  ( 0.000000000000000000, -0.000000000000000000, -1.000000000000000000 ) ) ;
#4704 = DIRECTION ( 'NONE',  ( 0.2853335501257686646, -0.9584282785752022971, 0.000000000000000000 ) ) ;
#4705 = LINE ( 'NONE', #7204, #1348 ) ;
#4706 = VERTEX_POINT ( 'NONE', #6109 ) ;
#4707 = EDGE_LOOP ( 'NONE', ( #1891, #6741, #1838, #3324, #4170, #2323, #7054, #4159, #4322 ) ) ;
#4708 = CARTESIAN_POINT ( 'NONE',  ( 6.190240298342080116, 0.4584752965317958062, 0.1250000000000000278 ) ) ;
#4709 = DIRECTION ( 'NONE',  ( -0.000000000000000000, -0.000000000000000000, 1.000000000000000000 ) ) ;
#4710 = DIRECTION ( 'NONE',  ( -1.000000000000000000, 0.000000000000000000, 0.000000000000000000 ) ) ;
#4711 = ORIENTED_EDGE ( 'NONE', *, *, #7480, .T. ) ;
#4712 = DIRECTION ( 'NONE',  ( -1.000000000000000000, 0.000000000000000000, -0.000000000000000000 ) ) ;
#4713 = DIRECTION ( 'NONE',  ( 0.000000000000000000, 1.000000000000000000, -0.000000000000000000 ) ) ;
#4714 = DIRECTION ( 'NONE',  ( -0.000000000000000000, -0.000000000000000000, -1.000000000000000000 ) ) ;
#4715 = PERSON_AND_ORGANIZATION ( #4735, #6190 ) ;
#4716 = ORIENTED_EDGE ( 'NONE', *, *, #125, .T. ) ;
#4717 = DIRECTION ( 'NONE',  ( 1.000000000000000000, 0.000000000000000000, 0.000000000000000000 ) ) ;
#4718 = FACE_OUTER_BOUND ( 'NONE', #2311, .T. ) ;
#4719 = EDGE_LOOP ( 'NONE', ( #5982, #6789, #2579, #2635 ) ) ;
#4720 = ORIENTED_EDGE ( 'NONE', *, *, #832, .T. ) ;
#4721 = EDGE_CURVE ( 'NONE', #4775, #2827, #4870, .T. ) ;
#4722 = VERTEX_POINT ( 'NONE', #2399 ) ;
#4723 = CARTESIAN_POINT ( 'NONE',  ( 1.872635725948145646, 1.428537503602546721, -0.05220482834521919524 ) ) ;
#4724 = CARTESIAN_POINT ( 'NONE',  ( -1.045535649164317071, -0.7375897546243017633, 0.004036567931050074297 ) ) ;
#4725 = PERSON_AND_ORGANIZATION_ROLE ( 'classification_officer' ) ;
#4726 = DIRECTION ( 'NONE',  ( -0.6157549048526803626, 0.7879377495398141029, -0.000000000000000000 ) ) ;
#4727 = ORIENTED_EDGE ( 'NONE', *, *, #3260, .F. ) ;
#4728 = APPLICATION_CONTEXT ( 'configuration controlled 3d designs of mechanical parts and assemblies' ) ;
#4729 = ORIENTED_EDGE ( 'NONE', *, *, #6046, .T. ) ;
#4730 = ORIENTED_EDGE ( 'NONE', *, *, #7588, .F. ) ;
#4731 = PRODUCT_DEFINITION_SHAPE ( 'NONE', 'NONE',  #8092 ) ;
#4732 = ORIENTED_EDGE ( 'NONE', *, *, #3601, .T. ) ;
#4733 = EDGE_CURVE ( 'NONE', #6342, #6542, #1243, .T. ) ;
#4734 = EDGE_CURVE ( 'NONE', #4105, #3222, #461, .T. ) ;
#4735 = PERSON ( 'UNSPECIFIED', 'UNSPECIFIED', 'UNSPECIFIED', ('UNSPECIFIED'), ('UNSPECIFIED'), ('UNSPECIFIED') ) ;
#4736 = CYLINDRICAL_SURFACE ( 'NONE', #6216, 0.3099999999999745737 ) ;
#4737 = ADVANCED_FACE ( 'NONE', ( #66 ), #7453, .T. ) ;
#4738 = EDGE_CURVE ( 'NONE', #2029, #6037, #2551, .T. ) ;
#4739 = CARTESIAN_POINT ( 'NONE',  ( 3.659299226295303686, -8.245510427152350275, -0.1849999999999999978 ) ) ;
#4740 = CARTESIAN_POINT ( 'NONE',  ( 1.492904096916551460, 1.856349440303736831, -0.001813861035895662039 ) ) ;
#4741 = ORIENTED_EDGE ( 'NONE', *, *, #5789, .T. ) ;
#4742 = APPROVAL ( #3912, 'UNSPECIFIED' ) ;
#4743 = DIRECTION ( 'NONE',  ( 1.000000000000000000, 0.000000000000000000, -0.000000000000000000 ) ) ;
#4744 = ADVANCED_FACE ( 'NONE', ( #1798 ), #1175, .F. ) ;
#4745 = DIRECTION ( 'NONE',  ( 1.000000000000000000, 0.000000000000000000, 0.000000000000000000 ) ) ;
#4746 = CC_DESIGN_SECURITY_CLASSIFICATION ( #418, ( #1857 ) ) ;
#4747 = EDGE_CURVE ( 'NONE', #2895, #5391, #5172, .T. ) ;
#4748 = VECTOR ( 'NONE', #1585, 39.37007874015748143 ) ;
#4749 = APPROVAL_PERSON_ORGANIZATION ( #5680, #2036, #5229 ) ;
#4750 = CARTESIAN_POINT ( 'NONE',  ( 0.09537553527426730071, -0.4271221084841553273, 0.2500000000000000000 ) ) ;
#4751 = CC_DESIGN_APPROVAL ( #4591, ( #7594 ) ) ;
#4752 = CARTESIAN_POINT ( 'NONE',  ( -6.110602001756019419, -1.404684638105634820, -0.05999999999999999778 ) ) ;
#4753 = CARTESIAN_POINT ( 'NONE',  ( 0.3517695222503834374, -0.3450570238940762757, 0.01951625562141530781 ) ) ;
#4754 = ORIENTED_EDGE ( 'NONE', *, *, #1273, .F. ) ;
#4755 = VECTOR ( 'NONE', #2053, 39.37007874015748143 ) ;
#4756 = CARTESIAN_POINT ( 'NONE',  ( -0.09999999999999997780, -0.03125000000000000000, 0.06250000000000000000 ) ) ;
#4757 = AXIS2_PLACEMENT_3D ( 'NONE', #6350, #7492, #768 ) ;
#4758 = CARTESIAN_POINT ( 'NONE',  ( -1.204376266962890796, -0.2040480809676099017, 0.03199999999999999373 ) ) ;
#4759 = DIRECTION ( 'NONE',  ( 0.000000000000000000, 0.000000000000000000, -1.000000000000000000 ) ) ;
#4760 = APPROVAL_ROLE ( '' ) ;
#4761 = VERTEX_POINT ( 'NONE', #6919 ) ;
#4762 = CARTESIAN_POINT ( 'NONE',  ( -0.1255000000000000282, 0.000000000000000000, -0.6229999999999998872 ) ) ;
#4763 = CARTESIAN_POINT ( 'NONE',  ( 1.492515782973968363, 1.856045982048426746, -0.05383208248535607116 ) ) ;
#4764 = CARTESIAN_POINT ( 'NONE',  ( 0.1250000000000000000, 0.5625000000000000000, -0.03125000000000000000 ) ) ;
#4765 = AXIS2_PLACEMENT_3D ( 'NONE', #1571, #2879, #2805 ) ;
#4766 =( BOUNDED_CURVE ( )  B_SPLINE_CURVE ( 3, ( #4594, #7094, #7746, #3980 ),
 .UNSPECIFIED., .F., .T. ) 
 B_SPLINE_CURVE_WITH_KNOTS ( ( 4, 4 ),
 ( 3.481429563043914932, 4.712388980384689674 ),
 .UNSPECIFIED. ) 
 CURVE ( )  GEOMETRIC_REPRESENTATION_ITEM ( )  RATIONAL_B_SPLINE_CURVE ( ( 1.000000000000000000, 0.8776643872851506156, 0.8776643872851506156, 1.000000000000000000 ) ) 
 REPRESENTATION_ITEM ( '' )  );
#4767 = ORIENTED_EDGE ( 'NONE', *, *, #7481, .T. ) ;
#4768 = AXIS2_PLACEMENT_3D ( 'NONE', #3800, #6785, #1166 ) ;
#4769 = VERTEX_POINT ( 'NONE', #1297 ) ;
#4770 = CARTESIAN_POINT ( 'NONE',  ( 1.859928773101481303, 1.466967662321851718, -0.01415936195527345114 ) ) ;
#4771 = AXIS2_PLACEMENT_3D ( 'NONE', #5630, #95, #1939 ) ;
#4772 = DIRECTION ( 'NONE',  ( -0.04906492035527816598, 0.9987955914953420278, 0.000000000000000000 ) ) ;
#4773 = APPROVAL_ROLE ( '' ) ;
#4774 = DIRECTION ( 'NONE',  ( -0.000000000000000000, -1.000000000000000000, -0.000000000000000000 ) ) ;
#4775 = VERTEX_POINT ( 'NONE', #1832 ) ;
#4776 = CC_DESIGN_APPROVAL ( #5247, ( #3335 ) ) ;
#4777 = VECTOR ( 'NONE', #6435, 39.37007874015748143 ) ;
#4778 = DIRECTION ( 'NONE',  ( 0.000000000000000000, 0.000000000000000000, 1.000000000000000000 ) ) ;
#4779 = FACE_OUTER_BOUND ( 'NONE', #4262, .T. ) ;
#4780 = SHAPE_DEFINITION_REPRESENTATION ( #3496, #6436 ) ;
#4781 = DIRECTION ( 'NONE',  ( -1.000000000000000000, -1.224646799147353207E-16, 0.000000000000000000 ) ) ;
#4782 = VERTEX_POINT ( 'NONE', #6758 ) ;
#4783 = CLOSED_SHELL ( 'NONE', ( #4694, #2027, #1795, #3232, #3499, #2925, #483, #4744, #2468, #3835, #1429, #3739, #5948, #939, #4181, #7147, #3201, #521, #5001, #6938, #5087, #488, #3288, #3382, #3645, #4737, #1420, #1367, #6736, #5202, #2193, #886, #5530, #2883, #1527, #2724, #6305 ) ) ;
#4784 = VECTOR ( 'NONE', #1751, 39.37007874015748143 ) ;
#4785 = EDGE_LOOP ( 'NONE', ( #988, #699, #4139 ) ) ;
#4786 = EDGE_CURVE ( 'NONE', #2414, #6740, #6230, .T. ) ;
#4787 = DIRECTION ( 'NONE',  ( 0.000000000000000000, 0.000000000000000000, 1.000000000000000000 ) ) ;
#4788 = EDGE_CURVE ( 'NONE', #3415, #2344, #4128, .T. ) ;
#4789 = ORIENTED_EDGE ( 'NONE', *, *, #3891, .F. ) ;
#4790 = ADVANCED_FACE ( 'NONE', ( #2566 ), #1143, .F. ) ;
#4791 = PLANE ( 'NONE',  #4896 ) ;
#4792 = AXIS2_PLACEMENT_3D ( 'NONE', #785, #4563, #1940 ) ;
#4793 = EDGE_LOOP ( 'NONE', ( #5963, #5525, #6762, #3267 ) ) ;
#4794 = ADVANCED_FACE ( 'NONE', ( #4986 ), #5568, .T. ) ;
#4795 = CARTESIAN_POINT ( 'NONE',  ( 0.000000000000000000, 1.050000000000000044, 0.000000000000000000 ) ) ;
#4796 = DIRECTION ( 'NONE',  ( -1.224646799147353207E-16, 1.000000000000000000, 0.000000000000000000 ) ) ;
#4797 = VECTOR ( 'NONE', #3275, 39.37007874015748143 ) ;
#4798 = EDGE_CURVE ( 'NONE', #3124, #7143, #5614, .T. ) ;
#4799 = VERTEX_POINT ( 'NONE', #4263 ) ;
#4800 = DIRECTION ( 'NONE',  ( 0.000000000000000000, 0.000000000000000000, 1.000000000000000000 ) ) ;
#4801 = VECTOR ( 'NONE', #116, 39.37007874015748143 ) ;
#4802 = CIRCLE ( 'NONE', #7162, 0.03200000000000005618 ) ;
#4803 = ADVANCED_FACE ( 'NONE', ( #8010 ), #7486, .F. ) ;
#4804 = CIRCLE ( 'NONE', #1010, 0.03125000000000000694 ) ;
#4805 = DIRECTION ( 'NONE',  ( 0.7879377495398137699, 0.6157549048526804736, 0.000000000000000000 ) ) ;
#4806 = DIRECTION ( 'NONE',  ( 0.000000000000000000, 0.000000000000000000, -1.000000000000000000 ) ) ;
#4807 = APPROVAL_STATUS ( 'not_yet_approved' ) ;
#4808 = ORIENTED_EDGE ( 'NONE', *, *, #4734, .T. ) ;
#4809 = CARTESIAN_POINT ( 'NONE',  ( 2.055894902224925769, 1.230239508989321440, -0.08212881570848257207 ) ) ;
#4810 = VECTOR ( 'NONE', #5856, 39.37007874015748143 ) ;
#4811 = DIRECTION ( 'NONE',  ( -0.000000000000000000, -0.000000000000000000, -1.000000000000000000 ) ) ;
#4812 = CARTESIAN_POINT ( 'NONE',  ( 0.09374999999999998612, 1.148106374200643401E-17, -0.6849999999999999423 ) ) ;
#4813 = AXIS2_PLACEMENT_3D ( 'NONE', #1323, #3176, #7565 ) ;
#4814 = EDGE_LOOP ( 'NONE', ( #7124, #5451, #5152, #2843 ) ) ;
#4815 = VECTOR ( 'NONE', #6803, 39.37007874015748143 ) ;
#4816 =( NAMED_UNIT ( * ) PLANE_ANGLE_UNIT ( ) SI_UNIT ( $, .RADIAN. ) );
#4817 = EDGE_LOOP ( 'NONE', ( #7689, #6599, #4267, #2161, #2734, #1411, #1632, #4892, #7363, #6541, #7686, #7331 ) ) ;
#4818 = DIRECTION ( 'NONE',  ( -0.7540216022612855618, 0.6568496200222115888, 0.000000000000000000 ) ) ;
#4819 = PLANE ( 'NONE',  #2201 ) ;
#4820 = ITEM_DEFINED_TRANSFORMATION ( 'NONE', 'NONE', #3437,  #3555 ) ;
#4821 = DIRECTION ( 'NONE',  ( 0.7879377495398141029, 0.6157549048526801405, 0.000000000000000000 ) ) ;
#4822 = AXIS2_PLACEMENT_3D ( 'NONE', #3075, #1307, #5581 ) ;
#4823 = ORIENTED_EDGE ( 'NONE', *, *, #5849, .T. ) ;
#4824 = B_SPLINE_CURVE_WITH_KNOTS ( 'NONE', 3,
 ( #3814, #5156, #1511, #1630, #984, #5372 ),
 .UNSPECIFIED., .F., .F.,
 ( 4, 2, 4 ),
 ( 7.607273545336762758E-15, 0.0006113010686663716007, 0.001222602137325135788 ),
 .UNSPECIFIED. ) ;
#4825 = CARTESIAN_POINT ( 'NONE',  ( -0.1255000000000000282, 1.916572240665608148E-17, 0.1250000000000000000 ) ) ;
#4826 = CARTESIAN_POINT ( 'NONE',  ( -1.723766588794375387, 1.115324847714046497, -0.2959999999999997078 ) ) ;
#4827 = CARTESIAN_POINT ( 'NONE',  ( 1.640223930641419914, 1.235377681954054285, -0.08212881570848259982 ) ) ;
#4828 = SECURITY_CLASSIFICATION_LEVEL ( 'unclassified' ) ;
#4829 = CARTESIAN_POINT ( 'NONE',  ( 0.000000000000000000, 0.000000000000000000, 0.1250000000000000000 ) ) ;
#4830 = CARTESIAN_POINT ( 'NONE',  ( 3.690413561029368683, -8.374393170229348371, 0.1849999999999999978 ) ) ;
#4831 = CARTESIAN_POINT ( 'NONE',  ( 1.526921265547024120, 1.208805900097675856, 0.1840890058364192117 ) ) ;
#4832 = DIRECTION ( 'NONE',  ( -0.000000000000000000, -0.000000000000000000, -1.000000000000000000 ) ) ;
#4833 = EDGE_CURVE ( 'NONE', #4299, #1231, #4427, .T. ) ;
#4834 = PLANE ( 'NONE',  #2025 ) ;
#4835 = CARTESIAN_POINT ( 'NONE',  ( 0.6690408158126811555, -0.04637372973215107830, 0.07449999999999999678 ) ) ;
#4836 = CARTESIAN_POINT ( 'NONE',  ( 1.142655413120957197, 0.6307864494084283180, 0.03199999999999999373 ) ) ;
#4837 = VERTEX_POINT ( 'NONE', #6274 ) ;
#4838 = ORIENTED_EDGE ( 'NONE', *, *, #6093, .F. ) ;
#4839 = CARTESIAN_POINT ( 'NONE',  ( -0.06250000000000000000, 0.000000000000000000, -0.6537499999999999423 ) ) ;
#4840 = ADVANCED_FACE ( 'NONE', ( #26 ), #648, .T. ) ;
#4841 = EDGE_CURVE ( 'NONE', #6242, #5571, #2924, .T. ) ;
#4842 = DIRECTION ( 'NONE',  ( 0.000000000000000000, 0.000000000000000000, 1.000000000000000000 ) ) ;
#4843 = DIRECTION ( 'NONE',  ( 1.000000000000000000, 0.000000000000000000, 0.000000000000000000 ) ) ;
#4844 = DATE_AND_TIME ( #2338, #23 ) ;
#4845 = ORIENTED_EDGE ( 'NONE', *, *, #7393, .F. ) ;
#4846 = EDGE_CURVE ( 'NONE', #5314, #7717, #5419, .T. ) ;
#4847 = FACE_OUTER_BOUND ( 'NONE', #2722, .T. ) ;
#4848 = FACE_OUTER_BOUND ( 'NONE', #5701, .T. ) ;
#4849 = FACE_OUTER_BOUND ( 'NONE', #5898, .T. ) ;
#4850 = CC_DESIGN_PERSON_AND_ORGANIZATION_ASSIGNMENT ( #1997, #4506, ( #1857 ) ) ;
#4851 = EDGE_CURVE ( 'NONE', #7230, #2575, #6465, .T. ) ;
#4852 = ADVANCED_FACE ( 'NONE', ( #5734 ), #3264, .T. ) ;
#4853 = EDGE_LOOP ( 'NONE', ( #244, #6532, #4415, #2302 ) ) ;
#4854 = ORIENTED_EDGE ( 'NONE', *, *, #5739, .F. ) ;
#4855 = CARTESIAN_POINT ( 'NONE',  ( 0.000000000000000000, 1.425000000000000044, 0.000000000000000000 ) ) ;
#4856 = CARTESIAN_POINT ( 'NONE',  ( 0.04627948923991306168, -0.4636619226355729873, 0.2393213367346657128 ) ) ;
#4857 = CALENDAR_DATE ( 2026, 9, 10 ) ;
#4858 = DIRECTION ( 'NONE',  ( 0.000000000000000000, 0.000000000000000000, 1.000000000000000000 ) ) ;
#4859 = ORIENTED_EDGE ( 'NONE', *, *, #4533, .F. ) ;
#4860 = CARTESIAN_POINT ( 'NONE',  ( -0.6570132742846659379, -0.6068321365170168402, 0.000000000000000000 ) ) ;
#4861 = DIRECTION ( 'NONE',  ( -0.000000000000000000, -1.000000000000000000, -0.000000000000000000 ) ) ;
#4862 = CARTESIAN_POINT ( 'NONE',  ( 0.09906724953193619954, -0.4587982231398470834, 0.02730009524027248238 ) ) ;
#4863 = DATE_AND_TIME ( #6864, #3827 ) ;
#4864 = DIRECTION ( 'NONE',  ( -1.224646799147353207E-16, 1.000000000000000000, 0.000000000000000000 ) ) ;
#4865 = CARTESIAN_POINT ( 'NONE',  ( 0.000000000000000000, 0.000000000000000000, 0.000000000000000000 ) ) ;
#4866 = ORIENTED_EDGE ( 'NONE', *, *, #5386, .F. ) ;
#4867 = CARTESIAN_POINT ( 'NONE',  ( 1.603337854698916320, 1.200890287003202328, 0.1947064082056160772 ) ) ;
#4868 = CARTESIAN_POINT ( 'NONE',  ( 1.586137004846402077, 0.9037470550431118133, -0.1039999999999998287 ) ) ;
#4869 = ORIENTED_EDGE ( 'NONE', *, *, #5241, .T. ) ;
#4870 = LINE ( 'NONE', #7367, #4784 ) ;
#4871 = CARTESIAN_POINT ( 'NONE',  ( 0.1250000000000000278, 0.03125000000000000000, 0.06250000000000000000 ) ) ;
#4872 = CC_DESIGN_APPROVAL ( #2994, ( #7247 ) ) ;
#4873 = DIRECTION ( 'NONE',  ( 0.000000000000000000, -0.000000000000000000, 1.000000000000000000 ) ) ;
#4874 = ORIENTED_EDGE ( 'NONE', *, *, #4230, .F. ) ;
#4875 = ORIENTED_EDGE ( 'NONE', *, *, #2144, .F. ) ;
#4876 = DIRECTION ( 'NONE',  ( 0.7879377495398141029, 0.6157549048526800295, 0.000000000000000000 ) ) ;
#4877 = CC_DESIGN_APPROVAL ( #4698, ( #1211 ) ) ;
#4878 = DIRECTION ( 'NONE',  ( -0.6157549048526801405, 0.7879377495398142139, 0.000000000000000000 ) ) ;
#4879 = CARTESIAN_POINT ( 'NONE',  ( 0.000000000000000000, 0.6250000000000000000, 0.000000000000000000 ) ) ;
#4880 = APPROVAL_ROLE ( '' ) ;
#4881 = VERTEX_POINT ( 'NONE', #4617 ) ;
#4882 = AXIS2_PLACEMENT_3D ( 'NONE', #1643, #3531, #5418 ) ;
#4883 = PLANE ( 'NONE',  #5729 ) ;
#4884 = FACE_BOUND ( 'NONE', #7863, .T. ) ;
#4885 = VERTEX_POINT ( 'NONE', #6996 ) ;
#4886 = FACE_BOUND ( 'NONE', #85, .T. ) ;
#4887 = EDGE_CURVE ( 'NONE', #1856, #2327, #6730, .T. ) ;
#4888 = VECTOR ( 'NONE', #1376, 39.37007874015748143 ) ;
#4889 = ORIENTED_EDGE ( 'NONE', *, *, #5941, .F. ) ;
#4890 = CARTESIAN_POINT ( 'NONE',  ( 0.1250000000000000000, 1.530808498934191509E-17, 0.1250000000000000000 ) ) ;
#4891 =( NAMED_UNIT ( * ) PLANE_ANGLE_UNIT ( ) SI_UNIT ( $, .RADIAN. ) );
#4892 = ORIENTED_EDGE ( 'NONE', *, *, #280, .T. ) ;
#4893 = DIRECTION ( 'NONE',  ( 0.000000000000000000, -1.000000000000000000, 0.000000000000000000 ) ) ;
#4894 = CONTEXT_DEPENDENT_SHAPE_REPRESENTATION ( #8068, #7353 ) ;
#4895 = FACE_OUTER_BOUND ( 'NONE', #2378, .T. ) ;
#4896 = AXIS2_PLACEMENT_3D ( 'NONE', #2102, #7193, #887 ) ;
#4897 = AXIS2_PLACEMENT_3D ( 'NONE', #1908, #3217, #3829 ) ;
#4898 = VECTOR ( 'NONE', #3397, 39.37007874015748143 ) ;
#4899 = ORIENTED_EDGE ( 'NONE', *, *, #2423, .F. ) ;
#4900 = DIRECTION ( 'NONE',  ( -0.000000000000000000, 0.000000000000000000, -1.000000000000000000 ) ) ;
#4901 = DIRECTION ( 'NONE',  ( 1.000000000000000000, 0.000000000000000000, 0.000000000000000000 ) ) ;
#4902 = ORIENTED_EDGE ( 'NONE', *, *, #80, .F. ) ;
#4903 = CARTESIAN_POINT ( 'NONE',  ( 1.353740795342265546, 0.002292344206094486941, -0.1250000000000000000 ) ) ;
#4904 = COORDINATED_UNIVERSAL_TIME_OFFSET ( 0, 0, .AHEAD. ) ;
#4905 = FACE_OUTER_BOUND ( 'NONE', #5654, .T. ) ;
#4906 = DIRECTION ( 'NONE',  ( 1.000000000000000000, 0.000000000000000000, 0.000000000000000000 ) ) ;
#4907 = VERTEX_POINT ( 'NONE', #1372 ) ;
#4908 = CARTESIAN_POINT ( 'NONE',  ( 1.486276370885186937, 1.194002588456842373, 0.1672982580699348132 ) ) ;
#4909 = DIRECTION ( 'NONE',  ( -0.6568496200222107007, -0.7540216022612862279, 0.000000000000000000 ) ) ;
#4910 = AXIS2_PLACEMENT_3D ( 'NONE', #4638, #3798, #6483 ) ;
#4911 = ORIENTED_EDGE ( 'NONE', *, *, #6931, .F. ) ;
#4912 = AXIS2_PLACEMENT_3D ( 'NONE', #5074, #6795, #7411 ) ;
#4913 = DIRECTION ( 'NONE',  ( 0.000000000000000000, 0.000000000000000000, -1.000000000000000000 ) ) ;
#4914 = CARTESIAN_POINT ( 'NONE',  ( 1.301886230480333584, 1.067115050693573819, -0.09588550097992007415 ) ) ;
#4915 = DIRECTION ( 'NONE',  ( 0.000000000000000000, -0.000000000000000000, 1.000000000000000000 ) ) ;
#4916 = ORIENTED_EDGE ( 'NONE', *, *, #2422, .F. ) ;
#4917 = EDGE_LOOP ( 'NONE', ( #6334, #6834, #6439, #6607 ) ) ;
#4918 = LINE ( 'NONE', #7417, #3316 ) ;
#4919 = CIRCLE ( 'NONE', #4792, 0.03124999999999997224 ) ;
#4920 = FACE_BOUND ( 'NONE', #8019, .T. ) ;
#4921 = CARTESIAN_POINT ( 'NONE',  ( 0.000000000000000000, 1.425000000000000044, 0.000000000000000000 ) ) ;
#4922 = AXIS2_PLACEMENT_3D ( 'NONE', #2910, #8021, #4967 ) ;
#4923 = APPROVAL_ROLE ( '' ) ;
#4924 = ORIENTED_EDGE ( 'NONE', *, *, #4143, .F. ) ;
#4925 = DIRECTION ( 'NONE',  ( 0.000000000000000000, -1.000000000000000000, 0.000000000000000000 ) ) ;
#4926 = CARTESIAN_POINT ( 'NONE',  ( 2.023273750469992349E-18, -0.03125000000000000000, 0.2731068805941697653 ) ) ;
#4927 = EDGE_LOOP ( 'NONE', ( #2515, #1237, #7452 ) ) ;
#4928 = VECTOR ( 'NONE', #6671, 39.37007874015748143 ) ;
#4929 = CARTESIAN_POINT ( 'NONE',  ( 0.1875000000000000278, 2.296212748401287726E-17, 0.06300000000000000044 ) ) ;
#4930 = AXIS2_PLACEMENT_3D ( 'NONE', #4177, #4796, #4957 ) ;
#4931 = AXIS2_PLACEMENT_3D ( 'NONE', #7727, #392, #5366 ) ;
#4932 = CIRCLE ( 'NONE', #6765, 0.1523203157102364369 ) ;
#4933 = CARTESIAN_POINT ( 'NONE',  ( 1.684866161243239846, 1.178252195112418299, -0.1039999999999998703 ) ) ;
#4934 = LENGTH_MEASURE_WITH_UNIT ( LENGTH_MEASURE( 0.02539999999999999897 ), #1486 );
#4935 = ADVANCED_FACE ( 'NONE', ( #5146 ), #6703, .T. ) ;
#4936 = DATE_AND_TIME ( #6815, #5164 ) ;
#4937 = CARTESIAN_POINT ( 'NONE',  ( 0.03125000000000000000, -0.03125000000000000000, -0.1162848326531996102 ) ) ;
#4938 = EDGE_CURVE ( 'NONE', #4722, #1300, #2010, .T. ) ;
#4939 = ORIENTED_EDGE ( 'NONE', *, *, #3338, .F. ) ;
#4940 = CIRCLE ( 'NONE', #1654, 0.2149999999999995803 ) ;
#4941 = CARTESIAN_POINT ( 'NONE',  ( -0.1250000000000000000, 0.5625000000000000000, -0.03125000000000000000 ) ) ;
#4942 = CARTESIAN_POINT ( 'NONE',  ( -1.499610808650658100, -1.013166758633947007, -0.05999999999999999778 ) ) ;
#4943 = EDGE_CURVE ( 'NONE', #7619, #6544, #1988, .T. ) ;
#4945 = CARTESIAN_POINT ( 'NONE',  ( -0.03921911030312474900, -0.4592703903598064352, 0.000000000000000000 ) ) ;
#4944 = VECTOR ( 'NONE', #6650, 39.37007874015748143 ) ;
#4946 = DATE_AND_TIME ( #2473, #3707 ) ;
#4947 = CARTESIAN_POINT ( 'NONE',  ( 0.8135394388118154518, 1.284829519253825492, -0.3750000000000000555 ) ) ;
#4948 = DIRECTION ( 'NONE',  ( 0.000000000000000000, 0.000000000000000000, -1.000000000000000000 ) ) ;
#4949 = EDGE_CURVE ( 'NONE', #5391, #502, #3977, .T. ) ;
#4950 = CARTESIAN_POINT ( 'NONE',  ( 1.657918913468165778, 1.341234511226818471, 0.2362032458804501078 ) ) ;
#4951 = DIMENSIONAL_EXPONENTS ( 1.000000000000000000, 0.000000000000000000, 0.000000000000000000, 0.000000000000000000, 0.000000000000000000, 0.000000000000000000, 0.000000000000000000 ) ;
#4952 = APPROVAL ( #1265, 'UNSPECIFIED' ) ;
#4953 = EDGE_CURVE ( 'NONE', #4276, #4688, #1016, .T. ) ;
#4954 = ORIENTED_EDGE ( 'NONE', *, *, #2986, .F. ) ;
#4955 = CARTESIAN_POINT ( 'NONE',  ( -1.855136387357835481, 0.9645206712600612464, -0.08100000000000007194 ) ) ;
#4956 = DIRECTION ( 'NONE',  ( 0.000000000000000000, 0.000000000000000000, 1.000000000000000000 ) ) ;
#4957 = DIRECTION ( 'NONE',  ( -1.000000000000000000, -1.224646799147353207E-16, 0.000000000000000000 ) ) ;
#4958 = ORIENTED_EDGE ( 'NONE', *, *, #728, .F. ) ;
#4959 = VERTEX_POINT ( 'NONE', #976 ) ;
#4960 = DIRECTION ( 'NONE',  ( -1.000000000000000000, -8.814117244050663918E-16, 0.000000000000000000 ) ) ;
#4961 = ORIENTED_EDGE ( 'NONE', *, *, #374, .F. ) ;
#4962 = SPHERICAL_SURFACE ( 'NONE', #2291, 0.01652128394798136474 ) ;
#4963 = CARTESIAN_POINT ( 'NONE',  ( -1.723766588794375387, 1.115324847714046497, -0.08100000000000007194 ) ) ;
#4964 = SECURITY_CLASSIFICATION_LEVEL ( 'unclassified' ) ;
#4965 = ORIENTED_EDGE ( 'NONE', *, *, #3027, .F. ) ;
#4966 = DIRECTION ( 'NONE',  ( 0.000000000000000000, 0.000000000000000000, -1.000000000000000000 ) ) ;
#4967 = DIRECTION ( 'NONE',  ( 0.000000000000000000, 0.000000000000000000, 1.000000000000000000 ) ) ;
#4968 = CARTESIAN_POINT ( 'NONE',  ( -1.750746777110393282, 1.631196835986985505, -0.05999999999999999778 ) ) ;
#4969 = CARTESIAN_POINT ( 'NONE',  ( -0.1250000000000000000, 0.6250000000000000000, -0.03125000000000000000 ) ) ;
#4970 = LENGTH_MEASURE_WITH_UNIT ( LENGTH_MEASURE( 0.02539999999999999897 ), #3665 );
#4971 = DIRECTION ( 'NONE',  ( 0.6157549048526801405, -0.7879377495398142139, -0.000000000000000000 ) ) ;
#4972 = COORDINATED_UNIVERSAL_TIME_OFFSET ( 0, 0, .AHEAD. ) ;
#4973 = DIRECTION ( 'NONE',  ( 1.000000000000000000, 0.000000000000000000, 0.000000000000000000 ) ) ;
#4974 = VERTEX_POINT ( 'NONE', #2889 ) ;
#4975 = ORIENTED_EDGE ( 'NONE', *, *, #5900, .T. ) ;
#4976 = CARTESIAN_POINT ( 'NONE',  ( 1.313749575516037105, 1.070113901150813174, -0.07404765044330269275 ) ) ;
#4977 = FACE_OUTER_BOUND ( 'NONE', #8045, .T. ) ;
#4978 = CARTESIAN_POINT ( 'NONE',  ( 1.475891671935536609, 0.7226544316391472211, -0.1849999999999999978 ) ) ;
#4979 = PERSON_AND_ORGANIZATION ( #4735, #6190 ) ;
#4980 = FACE_OUTER_BOUND ( 'NONE', #1495, .T. ) ;
#4981 = VERTEX_POINT ( 'NONE', #5934 ) ;
#4982 = CARTESIAN_POINT ( 'NONE',  ( 1.684660674153190429, 1.329988278726413009, 0.1880212863749382568 ) ) ;
#4983 = ADVANCED_FACE ( 'NONE', ( #7201 ), #6625, .T. ) ;
#4984 = ADVANCED_FACE ( 'NONE', ( #4124 ), #6051, .T. ) ;
#4985 = VERTEX_POINT ( 'NONE', #357 ) ;
#4986 = FACE_OUTER_BOUND ( 'NONE', #2800, .T. ) ;
#4987 = FACE_BOUND ( 'NONE', #2892, .T. ) ;
#4988 = EDGE_CURVE ( 'NONE', #7063, #6859, #6555, .T. ) ;
#4989 = EDGE_CURVE ( 'NONE', #1086, #7112, #1485, .T. ) ;
#4990 = CARTESIAN_POINT ( 'NONE',  ( 0.1210307295689817680, 0.6250000000000000000, 0.03125000000000000000 ) ) ;
#4991 = ORIENTED_EDGE ( 'NONE', *, *, #6003, .T. ) ;
#4992 = B_SPLINE_CURVE_WITH_KNOTS ( 'NONE', 3,
 ( #7177, #812, #5819, #863, #1590, #2091, #6479, #6562, #4753, #3368, #7086, #7251 ),
 .UNSPECIFIED., .F., .F.,
 ( 4, 2, 2, 2, 2, 4 ),
 ( 0.000000000000000000, 0.0005385383678279382193, 0.001077076735655876439, 0.001615615103483814983, 0.001884884287397780786, 0.002154153471311746806 ),
 .UNSPECIFIED. ) ;
#4993 = CARTESIAN_POINT ( 'NONE',  ( 0.1250000000000000278, 0.03125000000000000000, 0.000000000000000000 ) ) ;
#4994 = DIMENSIONAL_EXPONENTS ( 1.000000000000000000, 0.000000000000000000, 0.000000000000000000, 0.000000000000000000, 0.000000000000000000, 0.000000000000000000, 0.000000000000000000 ) ;
#4995 = ORIENTED_EDGE ( 'NONE', *, *, #7234, .F. ) ;
#4996 = CARTESIAN_POINT ( 'NONE',  ( 1.748556056214748189, 1.384842366659678081, 0.1776433458945842758 ) ) ;
#4997 = FACE_OUTER_BOUND ( 'NONE', #4531, .T. ) ;
#4998 = MECHANICAL_CONTEXT ( 'NONE', #1637, 'mechanical' ) ;
#4999 = ORIENTED_EDGE ( 'NONE', *, *, #3180, .T. ) ;
#5000 = CARTESIAN_POINT ( 'NONE',  ( 0.1250000000000000278, -0.03125000000000000000, 0.06250000000000000000 ) ) ;
#5001 = ADVANCED_FACE ( 'NONE', ( #5395, #2816 ), #6016, .T. ) ;
#5002 = CARTESIAN_POINT ( 'NONE',  ( -0.9280291358773672394, 0.8548654847802351631, 0.1250000000000000000 ) ) ;
#5003 = AXIS2_PLACEMENT_3D ( 'NONE', #6825, #2477, #5784 ) ;
#5004 = VERTEX_POINT ( 'NONE', #6097 ) ;
#5005 = CARTESIAN_POINT ( 'NONE',  ( 1.556400554713971651, 1.293514327272109687, 0.2500000000000000000 ) ) ;
#5006 = LOCAL_TIME ( 14, 45, 32.00000000000000000, #7321 ) ;
#5007 = ORIENTED_EDGE ( 'NONE', *, *, #6952, .T. ) ;
#5008 = VECTOR ( 'NONE', #4313, 39.37007874015748143 ) ;
#5009 = DIRECTION ( 'NONE',  ( -0.000000000000000000, -0.000000000000000000, -1.000000000000000000 ) ) ;
#5010 = CARTESIAN_POINT ( 'NONE',  ( 1.413441772008046993, 1.058152734179773402, -0.2027185361817280818 ) ) ;
#5011 = CARTESIAN_POINT ( 'NONE',  ( 0.000000000000000000, 0.000000000000000000, 0.09374999999999998612 ) ) ;
#5012 = EDGE_LOOP ( 'NONE', ( #4523, #6992, #7388, #881, #6896, #5409, #3765, #2288, #3351 ) ) ;
#5013 = ORIENTED_EDGE ( 'NONE', *, *, #1320, .F. ) ;
#5014 = CARTESIAN_POINT ( 'NONE',  ( 0.000000000000000000, 0.000000000000000000, -0.5599999999999999423 ) ) ;
#5015 = CARTESIAN_POINT ( 'NONE',  ( -1.050138139902704104, -0.7221301030214424266, 0.2500000000000000000 ) ) ;
#5016 = AXIS2_PLACEMENT_3D ( 'NONE', #3233, #2644, #3848 ) ;
#5017 = FACE_BOUND ( 'NONE', #651, .T. ) ;
#5018 = CALENDAR_DATE ( 2026, 9, 10 ) ;
#5019 = CARTESIAN_POINT ( 'NONE',  ( -1.479329383613507964, -3.808562985511015242, 0.2179999999999999993 ) ) ;
#5020 = CARTESIAN_POINT ( 'NONE',  ( 1.763818185482656009, 1.565523235941175928, -0.07053674507809003236 ) ) ;
#5021 = ORIENTED_EDGE ( 'NONE', *, *, #2611, .T. ) ;
#5022 = AXIS2_PLACEMENT_3D ( 'NONE', #1953, #3880, #6382 ) ;
#5023 = VECTOR ( 'NONE', #4832, 39.37007874015748143 ) ;
#5024 = SHAPE_REPRESENTATION ( 'Cleco, Fastener, Pincher', ( #3555 ), #553 ) ;
#5025 = ORIENTED_EDGE ( 'NONE', *, *, #8024, .F. ) ;
#5026 = CARTESIAN_POINT ( 'NONE',  ( -0.6570132742846659379, -0.6068321365170168402, 0.03200000000000000067 ) ) ;
#5027 = CARTESIAN_POINT ( 'NONE',  ( 1.370061665056169886, 1.067877247819581488, -0.1419528184087927580 ) ) ;
#5028 = EDGE_CURVE ( 'NONE', #7063, #3946, #4085, .T. ) ;
#5029 = LOCAL_TIME ( 14, 45, 32.00000000000000000, #259 ) ;
#5030 = EDGE_CURVE ( 'NONE', #7385, #1645, #5323, .T. ) ;
#5031 = EDGE_CURVE ( 'NONE', #4493, #2946, #1234, .T. ) ;
#5032 = AXIS2_PLACEMENT_3D ( 'NONE', #847, #6993, #3182 ) ;
#5033 = FACE_OUTER_BOUND ( 'NONE', #3529, .T. ) ;
#5034 = ORIENTED_EDGE ( 'NONE', *, *, #1424, .F. ) ;
#5035 = DIRECTION ( 'NONE',  ( 1.000000000000000000, 0.000000000000000000, 0.000000000000000000 ) ) ;
#5036 = EDGE_LOOP ( 'NONE', ( #5256, #1387, #6895, #1190 ) ) ;
#5037 = VECTOR ( 'NONE', #3832, 39.37007874015748143 ) ;
#5038 = CC_DESIGN_PERSON_AND_ORGANIZATION_ASSIGNMENT ( #1808, #5533, ( #7672 ) ) ;
#5039 = AXIS2_PLACEMENT_3D ( 'NONE', #401, #7822, #1715 ) ;
#5040 = DIRECTION ( 'NONE',  ( 0.000000000000000000, -1.000000000000000000, 0.000000000000000000 ) ) ;
#5041 = CYLINDRICAL_SURFACE ( 'NONE', #2963, 0.1250000000000000000 ) ;
#5042 = PERSON_AND_ORGANIZATION ( #4735, #6190 ) ;
#5043 = EDGE_CURVE ( 'NONE', #1943, #6593, #1551, .T. ) ;
#5044 = ORIENTED_EDGE ( 'NONE', *, *, #4142, .T. ) ;
#5045 = CARTESIAN_POINT ( 'NONE',  ( 1.401772513120452590, 1.065994035405744000, -0.1940432220382501405 ) ) ;
#5046 = CARTESIAN_POINT ( 'NONE',  ( -1.204376266962890796, -0.2040480809676099017, 0.2179999999999999993 ) ) ;
#5047 = CIRCLE ( 'NONE', #6358, 0.01652128394798136474 ) ;
#5048 = AXIS2_PLACEMENT_3D ( 'NONE', #5687, #4300, #4913 ) ;
#5049 = ORIENTED_EDGE ( 'NONE', *, *, #5896, .F. ) ;
#5050 = CARTESIAN_POINT ( 'NONE',  ( 3.672798492683009286, -8.252032378159654513, -0.1849999999999999978 ) ) ;
#5051 = CC_DESIGN_PERSON_AND_ORGANIZATION_ASSIGNMENT ( #5112, #7612, ( #1857 ) ) ;
#5052 = EDGE_CURVE ( 'NONE', #6392, #1869, #1753, .T. ) ;
#5053 = EDGE_CURVE ( 'NONE', #1476, #6638, #7169, .T. ) ;
#5054 = DIRECTION ( 'NONE',  ( -0.6157549048526801405, 0.7879377495398141029, 0.000000000000000000 ) ) ;
#5055 = DIRECTION ( 'NONE',  ( 0.000000000000000000, 0.000000000000000000, 1.000000000000000000 ) ) ;
#5056 = DIRECTION ( 'NONE',  ( 0.7879377495398139919, 0.6157549048526802515, 0.000000000000000000 ) ) ;
#5057 = CARTESIAN_POINT ( 'NONE',  ( -0.1210307295689817542, 0.6124999999999999334, 0.03125000000000000000 ) ) ;
#5058 = AXIS2_PLACEMENT_3D ( 'NONE', #2175, #7709, #4673 ) ;
#5059 = CIRCLE ( 'NONE', #1379, 0.2500000000000000555 ) ;
#5060 = VECTOR ( 'NONE', #1159, 39.37007874015748143 ) ;
#5061 = CARTESIAN_POINT ( 'NONE',  ( 1.846835003037430534, 1.498370261438588313, 0.000000000000000000 ) ) ;
#5062 = VERTEX_POINT ( 'NONE', #4055 ) ;
#5063 = CARTESIAN_POINT ( 'NONE',  ( 0.000000000000000000, 0.000000000000000000, -0.6849999999999999423 ) ) ;
#5064 = DATE_AND_TIME ( #6412, #1867 ) ;
#5065 = CARTESIAN_POINT ( 'NONE',  ( 1.302790242782180918, 1.667167568704493341, -0.1039999999999998703 ) ) ;
#5066 = DIRECTION ( 'NONE',  ( 0.000000000000000000, 1.000000000000000000, -0.000000000000000000 ) ) ;
#5067 = VERTEX_POINT ( 'NONE', #7277 ) ;
#5068 = VECTOR ( 'NONE', #1133, 39.37007874015748143 ) ;
#5069 = CIRCLE ( 'NONE', #6123, 0.1150000000000000050 ) ;
#5070 = AXIS2_PLACEMENT_3D ( 'NONE', #6985, #6332, #675 ) ;
#5071 = VECTOR ( 'NONE', #7945, 39.37007874015748143 ) ;
#5072 = FACE_OUTER_BOUND ( 'NONE', #4036, .T. ) ;
#5073 = ORIENTED_EDGE ( 'NONE', *, *, #4090, .F. ) ;
#5074 = CARTESIAN_POINT ( 'NONE',  ( 0.000000000000000000, 1.081250000000000044, 0.000000000000000000 ) ) ;
#5075 = DIRECTION ( 'NONE',  ( 0.000000000000000000, 0.000000000000000000, 1.000000000000000000 ) ) ;
#5076 = DIRECTION ( 'NONE',  ( -0.8875604078987042733, 0.4606913525677314158, 0.000000000000000000 ) ) ;
#5077 = FACE_OUTER_BOUND ( 'NONE', #5108, .T. ) ;
#5078 =( BOUNDED_SURFACE ( )  B_SPLINE_SURFACE ( 3, 2, ( 
 ( #3071, #5576, #2488 ),
 ( #4996, #7497, #4392 ),
 ( #1461, #806, #4060 ),
 ( #5903, #3270, #3235 ),
 ( #5155, #4624, #7005 ),
 ( #5771, #1381, #152 ),
 ( #4670, #279, #6474 ),
 ( #5740, #3893, #2648 ),
 ( #115, #2603, #7654 ),
 ( #1995, #771, #858 ),
 ( #734, #5110, #6426 ),
 ( #2044, #4025, #6388 ) ),
 .UNSPECIFIED., .F., .F., .F. ) 
 B_SPLINE_SURFACE_WITH_KNOTS ( ( 4, 2, 2, 2, 2, 4 ),
 ( 3, 3 ),
 ( 0.000000000000000000, 0.001544928261805478872, 0.002317392392708218091, 0.003089856523610957743, 0.004634784785416436181, 0.006179713047221915487 ),
 ( 0.000000000000000000, 1.000000000000000000 ),
 .UNSPECIFIED. ) 
 GEOMETRIC_REPRESENTATION_ITEM ( )  RATIONAL_B_SPLINE_SURFACE ( (
 ( 1.000000000000000000, 0.9155198504386535818, 1.000000000000000000),
 ( 1.000000000000000000, 0.9168944082009078400, 1.000000000000000000),
 ( 1.000000000000000000, 0.9178671560080209346, 1.000000000000000000),
 ( 1.000000000000000000, 0.9187365197604502320, 1.000000000000000000),
 ( 1.000000000000000000, 0.9189277564247825270, 1.000000000000000000),
 ( 1.000000000000000000, 0.9191098244346022073, 1.000000000000000000),
 ( 1.000000000000000000, 0.9190999940100047505, 1.000000000000000000),
 ( 1.000000000000000000, 0.9187630860089786022, 1.000000000000000000),
 ( 1.000000000000000000, 0.9181369762995320594, 1.000000000000000000),
 ( 1.000000000000000000, 0.9161154912244834359, 1.000000000000000000),
 ( 1.000000000000000000, 0.9147129675017228179, 1.000000000000000000),
 ( 1.000000000000000000, 0.9129308725696879678, 1.000000000000000000) ) ) 
 REPRESENTATION_ITEM ( '' )  SURFACE ( )  );
#5079 = DIRECTION ( 'NONE',  ( -0.000000000000000000, -0.000000000000000000, -1.000000000000000000 ) ) ;
#5080 = LINE ( 'NONE', #1996, #1646 ) ;
#5081 = APPROVAL_STATUS ( 'not_yet_approved' ) ;
#5082 = ORIENTED_EDGE ( 'NONE', *, *, #4135, .F. ) ;
#5083 = DIRECTION ( 'NONE',  ( 0.000000000000000000, 0.000000000000000000, -1.000000000000000000 ) ) ;
#5084 = CARTESIAN_POINT ( 'NONE',  ( 1.571814533976804151, 1.273076930690908437, 0.2372021369714001904 ) ) ;
#5085 = EDGE_CURVE ( 'NONE', #1943, #3663, #2205, .T. ) ;
#5086 = EDGE_CURVE ( 'NONE', #1110, #2261, #6585, .T. ) ;
#5087 = ADVANCED_FACE ( 'NONE', ( #4779 ), #7123, .T. ) ;
#5088 = CARTESIAN_POINT ( 'NONE',  ( 1.748511227875505725, 1.384809732886316702, 0.1776755382265015892 ) ) ;
#5089 = CARTESIAN_POINT ( 'NONE',  ( 0.000000000000000000, 0.000000000000000000, 0.000000000000000000 ) ) ;
#5090 = CARTESIAN_POINT ( 'NONE',  ( 0.2896281645421511231, -0.04777128394798136474, 0.000000000000000000 ) ) ;
#5091 = CARTESIAN_POINT ( 'NONE',  ( 1.492904096916551460, 1.856349440303736831, -0.001813861035895662039 ) ) ;
#5092 = ADVANCED_FACE ( 'NONE', ( #1658 ), #7919, .F. ) ;
#5093 = EDGE_CURVE ( 'NONE', #4537, #6252, #48, .T. ) ;
#5094 = ORIENTED_EDGE ( 'NONE', *, *, #2936, .T. ) ;
#5095 = ORIENTED_EDGE ( 'NONE', *, *, #5788, .F. ) ;
#5096 = CYLINDRICAL_SURFACE ( 'NONE', #1893, 0.1250000000000000000 ) ;
#5097 = SECURITY_CLASSIFICATION_LEVEL ( 'unclassified' ) ;
#5098 = DIRECTION ( 'NONE',  ( 0.6157549048526801405, -0.7879377495398139919, 0.000000000000000000 ) ) ;
#5099 = CARTESIAN_POINT ( 'NONE',  ( -6.110602001756019419, -1.404684638105634820, 0.3125000000000000000 ) ) ;
#5100 = ORIENTED_EDGE ( 'NONE', *, *, #7928, .T. ) ;
#5101 = ORIENTED_EDGE ( 'NONE', *, *, #576, .F. ) ;
#5102 = EDGE_LOOP ( 'NONE', ( #3424, #4607 ) ) ;
#5103 = LINE ( 'NONE', #4538, #2148 ) ;
#5104 = ORIENTED_EDGE ( 'NONE', *, *, #1624, .T. ) ;
#5105 = DIRECTION ( 'NONE',  ( -0.9987955914953421388, -0.04906492035527518225, 0.000000000000000000 ) ) ;
#5106 = DIRECTION ( 'NONE',  ( 0.000000000000000000, 0.000000000000000000, -1.000000000000000000 ) ) ;
#5107 = CARTESIAN_POINT ( 'NONE',  ( 1.260018307975525387, 1.633742302984369177, 0.2179999999999999993 ) ) ;
#5108 = EDGE_LOOP ( 'NONE', ( #3944, #3959, #5021, #6141, #2538 ) ) ;
#5109 = CARTESIAN_POINT ( 'NONE',  ( 0.1875000000000000278, 2.296212748401287726E-17, 0.06199999999999999956 ) ) ;
#5110 = CARTESIAN_POINT ( 'NONE',  ( 1.856253616992894262, 1.480980492019778438, 0.01345717186770836390 ) ) ;
#5111 = DIRECTION ( 'NONE',  ( -0.000000000000000000, 1.000000000000000000, -0.000000000000000000 ) ) ;
#5112 = PERSON_AND_ORGANIZATION ( #4735, #6190 ) ;
#5113 = ORIENTED_EDGE ( 'NONE', *, *, #3486, .F. ) ;
#5114 = CARTESIAN_POINT ( 'NONE',  ( 0.02822771919327313195, 0.03615965030275954117, 0.2500000000000000000 ) ) ;
#5115 = DIRECTION ( 'NONE',  ( 0.2791259188691606608, 0.9602545086670756236, 0.000000000000000000 ) ) ;
#5116 = VERTEX_POINT ( 'NONE', #7999 ) ;
#5117 = DIRECTION ( 'NONE',  ( -0.000000000000000000, -0.000000000000000000, -1.000000000000000000 ) ) ;
#5118 = LOCAL_TIME ( 14, 45, 32.00000000000000000, #1598 ) ;
#5119 = CARTESIAN_POINT ( 'NONE',  ( 0.000000000000000000, 0.000000000000000000, -0.6229999999999998872 ) ) ;
#5120 = CYLINDRICAL_SURFACE ( 'NONE', #711, 0.09904388296398869418 ) ;
#5121 = ADVANCED_FACE ( 'NONE', ( #5606 ), #7963, .T. ) ;
#5122 = CARTESIAN_POINT ( 'NONE',  ( -0.1250000000000000000, 0.000000000000000000, -0.1250000000000000000 ) ) ;
#5123 = EDGE_CURVE ( 'NONE', #3263, #5878, #3193, .T. ) ;
#5124 = VECTOR ( 'NONE', #173, 39.37007874015748143 ) ;
#5125 = DIRECTION ( 'NONE',  ( -0.000000000000000000, 1.000000000000000000, -0.000000000000000000 ) ) ;
#5126 = LOCAL_TIME ( 14, 45, 32.00000000000000000, #2437 ) ;
#5127 = EDGE_LOOP ( 'NONE', ( #1410, #1346, #6685, #2622 ) ) ;
#5128 = APPROVAL ( #5953, 'UNSPECIFIED' ) ;
#5129 = APPROVAL_PERSON_ORGANIZATION ( #5816, #2994, #1512 ) ;
#5130 = ORIENTED_EDGE ( 'NONE', *, *, #2995, .T. ) ;
#5131 = EDGE_CURVE ( 'NONE', #6877, #4612, #831, .T. ) ;
#5132 =( CONVERSION_BASED_UNIT ( 'INCH', #2554 ) LENGTH_UNIT ( ) NAMED_UNIT ( #2419 ) );
#5133 = CARTESIAN_POINT ( 'NONE',  ( 0.1054677083281892608, 0.5625000000000000000, 0.03125000000000000000 ) ) ;
#5134 = DATE_TIME_ROLE ( 'classification_date' ) ;
#5135 = LINE ( 'NONE', #2512, #7815 ) ;
#5136 = CARTESIAN_POINT ( 'NONE',  ( 2.387087291339119677, -6.013863021948615106, -0.1250000000000000000 ) ) ;
#5137 = AXIS2_PLACEMENT_3D ( 'NONE', #7582, #3321, #5821 ) ;
#5138 = ORIENTED_EDGE ( 'NONE', *, *, #8079, .F. ) ;
#5139 = VERTEX_POINT ( 'NONE', #3715 ) ;
#5140 = ORIENTED_EDGE ( 'NONE', *, *, #3231, .F. ) ;
#5141 = AXIS2_PLACEMENT_3D ( 'NONE', #360, #7701, #5285 ) ;
#5142 = ORIENTED_EDGE ( 'NONE', *, *, #3589, .F. ) ;
#5143 =( REPRESENTATION_RELATIONSHIP ('NONE','NONE', #3360, #4195 ) REPRESENTATION_RELATIONSHIP_WITH_TRANSFORMATION ( #6547 )SHAPE_REPRESENTATION_RELATIONSHIP( ) );
#5144 = FACE_BOUND ( 'NONE', #4599, .T. ) ;
#5145 = ORIENTED_EDGE ( 'NONE', *, *, #3825, .F. ) ;
#5146 = FACE_OUTER_BOUND ( 'NONE', #3503, .T. ) ;
#5147 = DIRECTION ( 'NONE',  ( -0.000000000000000000, -1.000000000000000000, -0.000000000000000000 ) ) ;
#5148 = CARTESIAN_POINT ( 'NONE',  ( -1.411633252941551175, 0.8434166392007488300, 0.1120558261758404089 ) ) ;
#5149 = ORIENTED_EDGE ( 'NONE', *, *, #5900, .F. ) ;
#5150 = VECTOR ( 'NONE', #4043, 39.37007874015748143 ) ;
#5151 = DIRECTION ( 'NONE',  ( 0.000000000000000000, 0.000000000000000000, -1.000000000000000000 ) ) ;
#5152 = ORIENTED_EDGE ( 'NONE', *, *, #3825, .T. ) ;
#5153 = AXIS2_PLACEMENT_3D ( 'NONE', #4602, #6330, #3948 ) ;
#5154 = AXIS2_PLACEMENT_3D ( 'NONE', #2379, #4893, #7389 ) ;
#5155 = CARTESIAN_POINT ( 'NONE',  ( 1.789066932586632630, 1.414966942634559466, 0.1362372702697500215 ) ) ;
#5156 = CARTESIAN_POINT ( 'NONE',  ( 1.535636747860705142, 1.849488204198513008, -0.03991733052746020138 ) ) ;
#5157 = DATE_AND_TIME ( #4027, #6578 ) ;
#5158 = LINE ( 'NONE', #197, #8035 ) ;
#5159 = CARTESIAN_POINT ( 'NONE',  ( -6.057578121783967262, -1.099253028489540318, 0.3125000000000000000 ) ) ;
#5160 = CARTESIAN_POINT ( 'NONE',  ( -1.204376266962895459, -0.2040480809675923046, 0.2266184113588085858 ) ) ;
#5161 = ORIENTED_EDGE ( 'NONE', *, *, #3285, .T. ) ;
#5162 = ORIENTED_EDGE ( 'NONE', *, *, #5250, .F. ) ;
#5163 = CARTESIAN_POINT ( 'NONE',  ( 1.452776126472616669, 1.185506347939969674, 0.2257575757582501175 ) ) ;
#5164 = LOCAL_TIME ( 14, 45, 32.00000000000000000, #6168 ) ;
#5165 = AXIS2_PLACEMENT_3D ( 'NONE', #3979, #4184, #5994 ) ;
#5166 = EDGE_LOOP ( 'NONE', ( #2447, #20, #6569, #2727 ) ) ;
#5167 = LINE ( 'NONE', #7181, #4387 ) ;
#5168 = DIRECTION ( 'NONE',  ( -0.6157549048526775870, 0.7879377495398161013, 0.000000000000000000 ) ) ;
#5169 = AXIS2_PLACEMENT_3D ( 'NONE', #6915, #4948, #3803 ) ;
#5170 = CARTESIAN_POINT ( 'NONE',  ( -2.290684594132797791, -0.9654407352564655653, 0.5227670380269011652 ) ) ;
#5171 = DIRECTION ( 'NONE',  ( -0.000000000000000000, -0.000000000000000000, -1.000000000000000000 ) ) ;
#5172 = CIRCLE ( 'NONE', #7142, 0.2149999999999995803 ) ;
#5173 = COORDINATED_UNIVERSAL_TIME_OFFSET ( 0, 0, .AHEAD. ) ;
#5174 = DIRECTION ( 'NONE',  ( 0.000000000000000000, 0.000000000000000000, -1.000000000000000000 ) ) ;
#5175 = CARTESIAN_POINT ( 'NONE',  ( 1.707875797406683382, 1.356648808867406020, 0.1757958501031237908 ) ) ;
#5176 = AXIS2_PLACEMENT_3D ( 'NONE', #3708, #1162, #465 ) ;
#5177 = EDGE_CURVE ( 'NONE', #2760, #3428, #2146, .T. ) ;
#5178 = ORIENTED_EDGE ( 'NONE', *, *, #231, .F. ) ;
#5179 = DIRECTION ( 'NONE',  ( -0.6157549048526804736, 0.7879377495398138809, 0.000000000000000000 ) ) ;
#5180 = ORIENTED_EDGE ( 'NONE', *, *, #2725, .F. ) ;
#5181 = CARTESIAN_POINT ( 'NONE',  ( 0.000000000000000000, 0.000000000000000000, 0.2500000000000000000 ) ) ;
#5182 = PERSON_AND_ORGANIZATION ( #4735, #6190 ) ;
#5183 = DIRECTION ( 'NONE',  ( -0.7879377495398156572, -0.6157549048526781421, -0.000000000000000000 ) ) ;
#5184 = CARTESIAN_POINT ( 'NONE',  ( 2.587066363198783776E-17, 1.081250000000000044, -0.2112499999999999933 ) ) ;
#5185 = CIRCLE ( 'NONE', #5710, 0.1255000000000000282 ) ;
#5186 = VECTOR ( 'NONE', #6926, 39.37007874015748143 ) ;
#5187 = VERTEX_POINT ( 'NONE', #4903 ) ;
#5188 = TOROIDAL_SURFACE ( 'NONE', #744, 0.2812500000000000000, 0.03125000000000000000 ) ;
#5189 = AXIS2_PLACEMENT_3D ( 'NONE', #4836, #1674, #6672 ) ;
#5190 = ORIENTED_EDGE ( 'NONE', *, *, #5839, .T. ) ;
#5191 = EDGE_CURVE ( 'NONE', #158, #4569, #7772, .T. ) ;
#5192 = ADVANCED_FACE ( 'NONE', ( #7402 ), #6602, .F. ) ;
#5193 = VERTEX_POINT ( 'NONE', #6748 ) ;
#5194 = DIRECTION ( 'NONE',  ( 0.6157549048526803626, -0.7879377495398141029, 0.000000000000000000 ) ) ;
#5195 = ORIENTED_EDGE ( 'NONE', *, *, #1673, .T. ) ;
#5197 = CARTESIAN_POINT ( 'NONE',  ( 1.626707180952940757, 1.340852667824533828, 0.2408335960773365370 ) ) ;
#5196 = AXIS2_PLACEMENT_3D ( 'NONE', #8084, #432, #6177 ) ;
#5198 = CARTESIAN_POINT ( 'NONE',  ( 1.360014742459622283, 1.082108298560946924, -0.1573894072555728219 ) ) ;
#5199 = CIRCLE ( 'NONE', #4414, 7.490657474112464520 ) ;
#5200 = PRODUCT_RELATED_PRODUCT_CATEGORY ( 'detail', '', ( #7731 ) ) ;
#5201 = CYLINDRICAL_SURFACE ( 'NONE', #1072, 0.2499962251234248700 ) ;
#5202 = ADVANCED_FACE ( 'NONE', ( #3675 ), #546, .T. ) ;
#5203 = ORIENTED_EDGE ( 'NONE', *, *, #3688, .T. ) ;
#5204 = CARTESIAN_POINT ( 'NONE',  ( 0.000000000000000000, 0.000000000000000000, 0.000000000000000000 ) ) ;
#5205 = AXIS2_PLACEMENT_3D ( 'NONE', #5065, #5098, #6865 ) ;
#5206 = ORIENTED_EDGE ( 'NONE', *, *, #7231, .F. ) ;
#5207 = CARTESIAN_POINT ( 'NONE',  ( 1.436243482636471613, 1.812070496725654012, 0.1571406716987245322 ) ) ;
#5208 = DIRECTION ( 'NONE',  ( 0.000000000000000000, 1.000000000000000000, 0.000000000000000000 ) ) ;
#5209 = COORDINATED_UNIVERSAL_TIME_OFFSET ( 0, 0, .AHEAD. ) ;
#5210 = CARTESIAN_POINT ( 'NONE',  ( -0.09999999999999997780, 0.03125000000000000000, 0.8125000000000000000 ) ) ;
#5211 = DIRECTION ( 'NONE',  ( -0.1461403971093831466, -0.1142052990486720071, 0.9826495479070427308 ) ) ;
#5212 = CIRCLE ( 'NONE', #1665, 6.962657474112426748 ) ;
#5213 = AXIS2_PLACEMENT_3D ( 'NONE', #3293, #5840, #1403 ) ;
#5214 = DIRECTION ( 'NONE',  ( 0.000000000000000000, 0.000000000000000000, 1.000000000000000000 ) ) ;
#5215 = ORIENTED_EDGE ( 'NONE', *, *, #5298, .T. ) ;
#5216 = DIRECTION ( 'NONE',  ( 0.7540216022612861169, -0.6568496200222107007, 0.000000000000000000 ) ) ;
#5217 = EDGE_CURVE ( 'NONE', #112, #225, #6539, .T. ) ;
#5218 = B_SPLINE_CURVE_WITH_KNOTS ( 'NONE', 3,
 ( #2453, #1108, #2961, #3656, #4347, #4224, #7461, #2407, #5659, #1226 ),
 .UNSPECIFIED., .F., .F.,
 ( 4, 2, 2, 2, 4 ),
 ( 3.400456267939447610E-16, 0.001260256529112787184, 0.002520513058225234363, 0.003780769587337681759, 0.005041026116450128720 ),
 .UNSPECIFIED. ) ;
#5219 = DIRECTION ( 'NONE',  ( 9.649454429013018880E-17, 7.540822732871182162E-17, 1.000000000000000000 ) ) ;
#5220 = CARTESIAN_POINT ( 'NONE',  ( -0.1054677083281892608, 0.6124999999999999334, -0.03125000000000000000 ) ) ;
#5221 = APPROVAL_ROLE ( '' ) ;
#5222 = VERTEX_POINT ( 'NONE', #6266 ) ;
#5223 = DIRECTION ( 'NONE',  ( 0.000000000000000000, 0.000000000000000000, -1.000000000000000000 ) ) ;
#5224 = CARTESIAN_POINT ( 'NONE',  ( 0.1875000000000000278, 0.000000000000000000, -0.6229999999999998872 ) ) ;
#5225 = ORIENTED_EDGE ( 'NONE', *, *, #7342, .F. ) ;
#5226 = CARTESIAN_POINT ( 'NONE',  ( -0.7707523566748063493, 0.2111891706072714925, -0.2208252761633266448 ) ) ;
#5227 = DIRECTION ( 'NONE',  ( 8.881784197001252323E-16, 0.000000000000000000, 1.000000000000000000 ) ) ;
#5228 = CARTESIAN_POINT ( 'NONE',  ( 1.347111479062088626E-17, 0.000000000000000000, -0.1100000000000000006 ) ) ;
#5229 = APPROVAL_ROLE ( '' ) ;
#5230 = DIRECTION ( 'NONE',  ( 1.000000000000000000, 0.000000000000000000, 0.000000000000000000 ) ) ;
#5231 = DIRECTION ( 'NONE',  ( -0.000000000000000000, -0.000000000000000000, -1.000000000000000000 ) ) ;
#5232 = ORIENTED_EDGE ( 'NONE', *, *, #5992, .T. ) ;
#5233 = EDGE_LOOP ( 'NONE', ( #5567, #5385, #601, #5847, #5398 ) ) ;
#5234 = EDGE_LOOP ( 'NONE', ( #7159, #2129, #6073, #6197 ) ) ;
#5235 = ORIENTED_EDGE ( 'NONE', *, *, #1274, .F. ) ;
#5236 = VERTEX_POINT ( 'NONE', #6221 ) ;
#5237 = CARTESIAN_POINT ( 'NONE',  ( 0.1250000000000000000, 1.530808498934191509E-17, 0.000000000000000000 ) ) ;
#5238 = VERTEX_POINT ( 'NONE', #4978 ) ;
#5239 = CARTESIAN_POINT ( 'NONE',  ( 1.584487667996386184, 1.282940758005886028, 0.2375274927211854514 ) ) ;
#5240 = CARTESIAN_POINT ( 'NONE',  ( -4.882388066182494768, 5.670153330992220297, -0.05999999999999999778 ) ) ;
#5241 = EDGE_CURVE ( 'NONE', #4782, #4572, #5296, .T. ) ;
#5242 = LINE ( 'NONE', #6557, #2908 ) ;
#5243 = ADVANCED_FACE ( 'NONE', ( #2510, #5017 ), #7518, .F. ) ;
#5244 = EDGE_CURVE ( 'NONE', #3476, #7840, #6451, .T. ) ;
#5245 = CARTESIAN_POINT ( 'NONE',  ( 0.8923633780935225079, 0.7607014108325282908, 0.2500000000000000000 ) ) ;
#5246 = ADVANCED_FACE ( 'NONE', ( #4000 ), #1321, .F. ) ;
#5247 = APPROVAL ( #583, 'UNKNOWN' ) ;
#5248 = EDGE_CURVE ( 'NONE', #2855, #5686, #574, .T. ) ;
#5249 = CARTESIAN_POINT ( 'NONE',  ( 1.514313407472767103, 1.834334088849169486, 0.06856807959217657567 ) ) ;
#5250 = EDGE_CURVE ( 'NONE', #6429, #1576, #714, .T. ) ;
#5251 = CARTESIAN_POINT ( 'NONE',  ( 3.690413561029368683, -8.374393170229348371, 0.1250000000000000000 ) ) ;
#5252 = APPROVAL_ROLE ( '' ) ;
#5253 = DIRECTION ( 'NONE',  ( -0.6568496200222107007, -0.7540216022612863389, 0.000000000000000000 ) ) ;
#5254 = DIRECTION ( 'NONE',  ( 0.000000000000000000, 0.000000000000000000, 1.000000000000000000 ) ) ;
#5255 = DIRECTION ( 'NONE',  ( -0.000000000000000000, -0.000000000000000000, -1.000000000000000000 ) ) ;
#5256 = ORIENTED_EDGE ( 'NONE', *, *, #5241, .F. ) ;
#5257 = DIRECTION ( 'NONE',  ( -1.000000000000000000, 0.000000000000000000, 0.000000000000000000 ) ) ;
#5258 = DIRECTION ( 'NONE',  ( -0.6568496200222102566, 0.7540216022612866720, -0.000000000000000000 ) ) ;
#5259 = LINE ( 'NONE', #205, #7549 ) ;
#5260 = PERSON_AND_ORGANIZATION ( #4735, #6190 ) ;
#5261 = ORIENTED_EDGE ( 'NONE', *, *, #4949, .F. ) ;
#5262 = ORIENTED_EDGE ( 'NONE', *, *, #838, .F. ) ;
#5263 = FACE_OUTER_BOUND ( 'NONE', #2835, .T. ) ;
#5264 = PRODUCT_DEFINITION_SHAPE ( 'NONE', 'NONE',  #3600 ) ;
#5265 = CARTESIAN_POINT ( 'NONE',  ( 1.469438155933634249, 1.205893913485946767, 0.2500000000000000555 ) ) ;
#5266 = CC_DESIGN_APPROVAL ( #3691, ( #4083 ) ) ;
#5267 = DIRECTION ( 'NONE',  ( -1.000000000000000000, 0.000000000000000000, 0.000000000000000000 ) ) ;
#5268 = CIRCLE ( 'NONE', #1070, 0.06250000000000000000 ) ;
#5269 = APPROVAL_PERSON_ORGANIZATION ( #809, #89, #5252 ) ;
#5270 = CALENDAR_DATE ( 2026, 9, 10 ) ;
#5271 = DIRECTION ( 'NONE',  ( 1.000000000000000000, 0.000000000000000000, 0.000000000000000000 ) ) ;
#5272 = CARTESIAN_POINT ( 'NONE',  ( 1.780616048947831098, 1.055727875058976251, -0.08212881570848259982 ) ) ;
#5273 = ORIENTED_EDGE ( 'NONE', *, *, #336, .T. ) ;
#5274 = AXIS2_PLACEMENT_3D ( 'NONE', #7848, #6057, #2893 ) ;
#5275 = ORIENTED_EDGE ( 'NONE', *, *, #7043, .F. ) ;
#5276 = B_SPLINE_CURVE_WITH_KNOTS ( 'NONE', 3,
 ( #2840, #7753, #2142, #4648 ),
 .UNSPECIFIED., .F., .F.,
 ( 4, 4 ),
 ( 0.9794065391376511887, 1.000000000000000000 ),
 .UNSPECIFIED. ) ;
#5277 = VERTEX_POINT ( 'NONE', #4452 ) ;
#5278 = EDGE_LOOP ( 'NONE', ( #497, #3967 ) ) ;
#5279 = DIRECTION ( 'NONE',  ( 0.000000000000000000, 0.000000000000000000, -1.000000000000000000 ) ) ;
#5280 = EDGE_LOOP ( 'NONE', ( #4315, #5886, #1012, #6622 ) ) ;
#5281 = CARTESIAN_POINT ( 'NONE',  ( 1.699282386309489246, 1.352382324664254565, 0.2085298325956354282 ) ) ;
#5282 = FACE_OUTER_BOUND ( 'NONE', #2981, .T. ) ;
#5283 = CARTESIAN_POINT ( 'NONE',  ( 1.258616367985684104, -0.02482036785324303815, 0.1849999999999999978 ) ) ;
#5284 = ORIENTED_EDGE ( 'NONE', *, *, #679, .T. ) ;
#5285 = DIRECTION ( 'NONE',  ( -1.224646799147352961E-16, 0.000000000000000000, -1.000000000000000000 ) ) ;
#5286 = AXIS2_PLACEMENT_3D ( 'NONE', #3268, #6923, #7608 ) ;
#5287 = EDGE_CURVE ( 'NONE', #4799, #5830, #7903, .T. ) ;
#5288 = CARTESIAN_POINT ( 'NONE',  ( 1.458223839541642475, 1.829247631064747193, 0.1297679841924749000 ) ) ;
#5289 = DIRECTION ( 'NONE',  ( -0.6157549048526804736, 0.7879377495398138809, -0.000000000000000000 ) ) ;
#5290 = VECTOR ( 'NONE', #4213, 39.37007874015748143 ) ;
#5291 = CARTESIAN_POINT ( 'NONE',  ( 1.780616048947831986, 1.055727875058976917, -0.1039999999999998703 ) ) ;
#5292 = LINE ( 'NONE', #5868, #4020 ) ;
#5293 = VERTEX_POINT ( 'NONE', #3174 ) ;
#5294 = DIRECTION ( 'NONE',  ( -0.000000000000000000, -0.000000000000000000, -1.000000000000000000 ) ) ;
#5295 = ADVANCED_FACE ( 'NONE', ( #101 ), #5096, .F. ) ;
#5296 = CIRCLE ( 'NONE', #3849, 9.064497838702109789 ) ;
#5297 = EDGE_CURVE ( 'NONE', #1984, #1061, #7895, .T. ) ;
#5298 = EDGE_CURVE ( 'NONE', #1238, #3518, #2592, .T. ) ;
#5299 = CARTESIAN_POINT ( 'NONE',  ( 0.000000000000000000, 0.03125000000000000000, 0.6481068805941697653 ) ) ;
#5300 = CARTESIAN_POINT ( 'NONE',  ( 1.536996473476847536, 1.850194254987160836, -0.04789697820785929205 ) ) ;
#5301 = APPROVAL_ROLE ( '' ) ;
#5302 = ORIENTED_EDGE ( 'NONE', *, *, #1581, .T. ) ;
#5303 = EDGE_LOOP ( 'NONE', ( #3190, #1146, #3261, #1693 ) ) ;
#5304 = DIRECTION ( 'NONE',  ( 0.000000000000000000, -0.000000000000000000, 1.000000000000000000 ) ) ;
#5305 = ORGANIZATION ( 'NAUO-ORG9', 'UNSPECIFIED', 'UNSPECIFIED' ) ;
#5306 = CIRCLE ( 'NONE', #61, 0.2499962251234248700 ) ;
#5307 = CARTESIAN_POINT ( 'NONE',  ( 1.487965390510427088, 1.244492490061562817, 0.2500000000000000000 ) ) ;
#5308 = CC_DESIGN_DATE_AND_TIME_ASSIGNMENT ( #2578, #7007, ( #3600 ) ) ;
#5309 = ADVANCED_FACE ( 'NONE', ( #5679 ), #7597, .F. ) ;
#5310 = ORIENTED_EDGE ( 'NONE', *, *, #5787, .F. ) ;
#5311 = VECTOR ( 'NONE', #6018, 39.37007874015748143 ) ;
#5312 = AXIS2_PLACEMENT_3D ( 'NONE', #5484, #7970, #2356 ) ;
#5313 = DIRECTION ( 'NONE',  ( 3.467552612600062496E-13, 1.462163723431325863E-13, -1.000000000000000222 ) ) ;
#5314 = VERTEX_POINT ( 'NONE', #3255 ) ;
#5315 = CYLINDRICAL_SURFACE ( 'NONE', #6078, 0.03200000000000008393 ) ;
#5316 = DIRECTION ( 'NONE',  ( 0.000000000000000000, 1.000000000000000000, 0.000000000000000000 ) ) ;
#5317 = APPROVAL_STATUS ( 'not_yet_approved' ) ;
#5318 = FACE_OUTER_BOUND ( 'NONE', #5888, .T. ) ;
#5319 = EDGE_LOOP ( 'NONE', ( #2274, #5429 ) ) ;
#5320 = ORIENTED_EDGE ( 'NONE', *, *, #6921, .F. ) ;
#5321 = PLANE ( 'NONE',  #49 ) ;
#5322 = VECTOR ( 'NONE', #4811, 39.37007874015748143 ) ;
#5323 = LINE ( 'NONE', #7846, #4112 ) ;
#5324 = CARTESIAN_POINT ( 'NONE',  ( 1.355995127727091409, 1.749358286058404488, 0.2179999999999997218 ) ) ;
#5325 = DIRECTION ( 'NONE',  ( 1.000000000000000000, 0.000000000000000000, 0.000000000000000000 ) ) ;
#5326 = EDGE_LOOP ( 'NONE', ( #7725, #6277 ) ) ;
#5327 = LINE ( 'NONE', #7814, #3453 ) ;
#5328 = AXIS2_PLACEMENT_3D ( 'NONE', #1755, #6760, #6637 ) ;
#5329 = VECTOR ( 'NONE', #2944, 39.37007874015748143 ) ;
#5330 = TOROIDAL_SURFACE ( 'NONE', #354, 0.2704878104020024265, 0.03200000000000000067 ) ;
#5331 = PRODUCT_DEFINITION_SHAPE ( 'NONE', 'NONE',  #8093 ) ;
#5332 = CARTESIAN_POINT ( 'NONE',  ( 1.260018307975524943, 1.633742302984368733, 0.2499999999999998890 ) ) ;
#5333 = DIRECTION ( 'NONE',  ( 0.7540216022612865610, -0.6568496200222104786, 0.000000000000000000 ) ) ;
#5334 = DIRECTION ( 'NONE',  ( -0.000000000000000000, -0.000000000000000000, -1.000000000000000000 ) ) ;
#5335 = ORIENTED_EDGE ( 'NONE', *, *, #6506, .T. ) ;
#5336 = ADVANCED_BREP_SHAPE_REPRESENTATION ( '', ( #869, #3555 ), #2771 ) ;
#5337 = AXIS2_PLACEMENT_3D ( 'NONE', #3717, #8001, #7447 ) ;
#5338 = DIRECTION ( 'NONE',  ( 0.000000000000000000, 0.000000000000000000, -1.000000000000000000 ) ) ;
#5339 = EDGE_CURVE ( 'NONE', #7690, #1501, #7174, .T. ) ;
#5340 = AXIS2_PLACEMENT_3D ( 'NONE', #1660, #4169, #6664 ) ;
#5341 = LINE ( 'NONE', #6280, #3470 ) ;
#5342 = CIRCLE ( 'NONE', #6645, 9.064497838702109789 ) ;
#5343 = CARTESIAN_POINT ( 'NONE',  ( 3.659299226295303686, -8.245510427152350275, 0.1850000000000003586 ) ) ;
#5344 = APPROVAL_STATUS ( 'not_yet_approved' ) ;
#5345 = ORIENTED_EDGE ( 'NONE', *, *, #3179, .F. ) ;
#5346 = CARTESIAN_POINT ( 'NONE',  ( 0.000000000000000000, 0.000000000000000000, 0.1250000000000000000 ) ) ;
#5347 = CARTESIAN_POINT ( 'NONE',  ( 1.533242936008017532, 1.243109892254450344, 0.2356317254196890199 ) ) ;
#5348 = EDGE_CURVE ( 'NONE', #409, #24, #1400, .T. ) ;
#5349 = EDGE_CURVE ( 'NONE', #4985, #5803, #3641, .T. ) ;
#5350 = EDGE_CURVE ( 'NONE', #7484, #2220, #6369, .T. ) ;
#5351 = ORIENTED_EDGE ( 'NONE', *, *, #6513, .T. ) ;
#5352 = ORIENTED_EDGE ( 'NONE', *, *, #7938, .T. ) ;
#5353 = CC_DESIGN_DATE_AND_TIME_ASSIGNMENT ( #792, #5134, ( #5666 ) ) ;
#5354 = EDGE_CURVE ( 'NONE', #810, #7906, #6525, .T. ) ;
#5355 =( LENGTH_UNIT ( ) NAMED_UNIT ( * ) SI_UNIT ( $, .METRE. ) );
#5356 = VERTEX_POINT ( 'NONE', #5133 ) ;
#5357 = CARTESIAN_POINT ( 'NONE',  ( -1.983451234524918450, 1.341543513548241418, -0.2959999999999997078 ) ) ;
#5358 = CARTESIAN_POINT ( 'NONE',  ( 0.009770039481058666320, -0.4636495502210370989, 0.2461822072133919292 ) ) ;
#5359 = EDGE_CURVE ( 'NONE', #2759, #1645, #4524, .T. ) ;
#5360 = DATE_AND_TIME ( #1652, #3692 ) ;
#5361 = DIRECTION ( 'NONE',  ( -0.7879377495407453580, -0.6157549048514884271, 0.000000000000000000 ) ) ;
#5362 = VERTEX_POINT ( 'NONE', #3911 ) ;
#5363 = ORIENTED_EDGE ( 'NONE', *, *, #4690, .F. ) ;
#5364 = DIRECTION ( 'NONE',  ( 0.000000000000000000, 0.000000000000000000, -1.000000000000000000 ) ) ;
#5365 = CARTESIAN_POINT ( 'NONE',  ( 3.672798492683009286, -8.252032378159654513, 0.1850000000000003586 ) ) ;
#5366 = DIRECTION ( 'NONE',  ( 0.2791259188691606608, 0.9602545086670756236, 0.000000000000000000 ) ) ;
#5367 = EDGE_LOOP ( 'NONE', ( #4991, #895, #1302, #6550 ) ) ;
#5368 = CARTESIAN_POINT ( 'NONE',  ( 1.635022706329736897, 1.287156158165765563, 0.2002339888563465509 ) ) ;
#5369 = CARTESIAN_POINT ( 'NONE',  ( 0.000000000000000000, 0.000000000000000000, 0.1250000000000000000 ) ) ;
#5370 = ORIENTED_EDGE ( 'NONE', *, *, #2479, .T. ) ;
#5371 = CARTESIAN_POINT ( 'NONE',  ( -4.882388066182508091, 5.670153330992292240, 0.2500000000000000000 ) ) ;
#5372 = CARTESIAN_POINT ( 'NONE',  ( 1.537918127343594454, 1.852987194258524983, 0.000000000000000000 ) ) ;
#5373 = DIRECTION ( 'NONE',  ( 0.000000000000000000, 0.000000000000000000, -1.000000000000000000 ) ) ;
#5374 = VERTEX_POINT ( 'NONE', #5796 ) ;
#5375 = DIRECTION ( 'NONE',  ( 0.000000000000000000, 0.000000000000000000, -1.000000000000000000 ) ) ;
#5376 = CARTESIAN_POINT ( 'NONE',  ( 0.000000000000000000, 0.6124999999999999334, 0.000000000000000000 ) ) ;
#5377 = LINE ( 'NONE', #2795, #5071 ) ;
#5378 = CALENDAR_DATE ( 2026, 9, 10 ) ;
#5379 = ORIENTED_EDGE ( 'NONE', *, *, #215, .F. ) ;
#5380 = FACE_OUTER_BOUND ( 'NONE', #4295, .T. ) ;
#5381 = DIRECTION ( 'NONE',  ( 0.000000000000000000, 0.000000000000000000, -1.000000000000000000 ) ) ;
#5382 = VERTEX_POINT ( 'NONE', #2672 ) ;
#5383 = EDGE_CURVE ( 'NONE', #5676, #3956, #2717, .T. ) ;
#5384 = ADVANCED_FACE ( 'NONE', ( #2103 ), #1651, .T. ) ;
#5385 = ORIENTED_EDGE ( 'NONE', *, *, #2038, .F. ) ;
#5386 = EDGE_CURVE ( 'NONE', #3782, #4623, #2120, .T. ) ;
#5387 = PLANE ( 'NONE',  #7250 ) ;
#5388 = CARTESIAN_POINT ( 'NONE',  ( -1.047748016704662666, -0.7301584672333364390, 0.0008302559380426106136 ) ) ;
#5389 = APPROVAL_ROLE ( '' ) ;
#5390 = DIRECTION ( 'NONE',  ( 0.000000000000000000, 0.000000000000000000, -1.000000000000000000 ) ) ;
#5391 = VERTEX_POINT ( 'NONE', #258 ) ;
#5392 = CIRCLE ( 'NONE', #1854, 0.1204106507132265275 ) ;
#5393 = DIRECTION ( 'NONE',  ( -0.6157549048526804736, 0.7879377495398138809, 0.000000000000000000 ) ) ;
#5394 = DESIGN_CONTEXT ( 'detailed design', #702, 'design' ) ;
#5395 = FACE_OUTER_BOUND ( 'NONE', #4426, .T. ) ;
#5396 = MECHANICAL_CONTEXT ( 'NONE', #3900, 'mechanical' ) ;
#5397 = LINE ( 'NONE', #2272, #2191 ) ;
#5398 = ORIENTED_EDGE ( 'NONE', *, *, #7102, .F. ) ;
#5399 = DIRECTION ( 'NONE',  ( -0.000000000000000000, 1.000000000000000000, -0.000000000000000000 ) ) ;
#5400 = PLANE ( 'NONE',  #4241 ) ;
#5401 = APPROVAL_PERSON_ORGANIZATION ( #2454, #4341, #1341 ) ;
#5402 = PRODUCT_DEFINITION ( 'UNKNOWN', '', #7756, #4014 ) ;
#5403 = EDGE_LOOP ( 'NONE', ( #7490, #6882, #7723, #7161, #6924, #6225 ) ) ;
#5404 = SECURITY_CLASSIFICATION ( '', '', #7790 ) ;
#5405 = CYLINDRICAL_SURFACE ( 'NONE', #4008, 0.3243589946935200308 ) ;
#5406 = CC_DESIGN_APPROVAL ( #7495, ( #4480 ) ) ;
#5407 = CARTESIAN_POINT ( 'NONE',  ( 0.07000000000000002054, 0.03125000000000000000, 0.8125000000000000000 ) ) ;
#5408 = CARTESIAN_POINT ( 'NONE',  ( -0.1250000000000000000, 0.6250000000000000000, 0.03125000000000000000 ) ) ;
#5409 = ORIENTED_EDGE ( 'NONE', *, *, #1829, .F. ) ;
#5410 = VECTOR ( 'NONE', #5216, 39.37007874015748854 ) ;
#5411 = CYLINDRICAL_SURFACE ( 'NONE', #1742, 8.696493751522730520 ) ;
#5412 = CARTESIAN_POINT ( 'NONE',  ( -1.197351689389629881, -0.2276434618412936095, 0.0008144248133129071551 ) ) ;
#5413 = CARTESIAN_POINT ( 'NONE',  ( 1.490392939745680323, 1.854387029763408190, -0.03263051443878305091 ) ) ;
#5414 = PERSON_AND_ORGANIZATION ( #4735, #6190 ) ;
#5415 = VERTEX_POINT ( 'NONE', #4044 ) ;
#5416 = DIRECTION ( 'NONE',  ( 0.6157549048526775870, -0.7879377495398161013, 0.000000000000000000 ) ) ;
#5417 = LINE ( 'NONE', #7308, #600 ) ;
#5418 = DIRECTION ( 'NONE',  ( 1.000000000000000000, 0.000000000000000000, 0.000000000000000000 ) ) ;
#5419 = CIRCLE ( 'NONE', #3215, 0.03200000000000002148 ) ;
#5420 = CIRCLE ( 'NONE', #705, 0.03200000000000009781 ) ;
#5421 = ORIENTED_EDGE ( 'NONE', *, *, #3589, .T. ) ;
#5422 = CC_DESIGN_APPROVAL ( #2789, ( #2562 ) ) ;
#5423 = ORIENTED_EDGE ( 'NONE', *, *, #3344, .T. ) ;
#5424 = CARTESIAN_POINT ( 'NONE',  ( 0.000000000000000000, 1.425000000000000044, 0.1487499999999999933 ) ) ;
#5425 = CIRCLE ( 'NONE', #1895, 4.032000000000000917 ) ;
#5426 = CARTESIAN_POINT ( 'NONE',  ( 0.3566525292043913886, -0.3408511508279085667, 0.2179999999999999993 ) ) ;
#5427 = COORDINATED_UNIVERSAL_TIME_OFFSET ( 0, 0, .AHEAD. ) ;
#5428 = DIRECTION ( 'NONE',  ( -1.000000000000000000, 0.000000000000000000, 0.000000000000000000 ) ) ;
#5429 = ORIENTED_EDGE ( 'NONE', *, *, #4938, .F. ) ;
#5430 = AXIS2_PLACEMENT_3D ( 'NONE', #5376, #367, #1150 ) ;
#5431 = DIRECTION ( 'NONE',  ( 0.000000000000000000, 0.000000000000000000, -1.000000000000000000 ) ) ;
#5432 = DIRECTION ( 'NONE',  ( 0.000000000000000000, 0.000000000000000000, -1.000000000000000000 ) ) ;
#5433 = CARTESIAN_POINT ( 'NONE',  ( 0.000000000000000000, 0.03125000000000000000, 0.000000000000000000 ) ) ;
#5434 = PERSON_AND_ORGANIZATION_ROLE ( 'design_supplier' ) ;
#5435 = CARTESIAN_POINT ( 'NONE',  ( 1.843369769566449712, 1.222798067273466627, -0.1039999999999998703 ) ) ;
#5436 = DIRECTION ( 'NONE',  ( 0.000000000000000000, 1.000000000000000000, 0.000000000000000000 ) ) ;
#5437 = CIRCLE ( 'NONE', #2294, 0.3099999999999745737 ) ;
#5438 = AXIS2_PLACEMENT_3D ( 'NONE', #5531, #5040, #5702 ) ;
#5439 = VERTEX_POINT ( 'NONE', #4655 ) ;
#5440 = CARTESIAN_POINT ( 'NONE',  ( 1.506219191374974731, 1.199057446088450440, 0.1758031223993888059 ) ) ;
#5441 = DIRECTION ( 'NONE',  ( 1.000000000000000000, 0.000000000000000000, 0.000000000000000000 ) ) ;
#5442 = EDGE_CURVE ( 'NONE', #5238, #4885, #1572, .T. ) ;
#5443 = AXIS2_PLACEMENT_3D ( 'NONE', #6087, #5508, #4973 ) ;
#5444 = ORIENTED_EDGE ( 'NONE', *, *, #7440, .F. ) ;
#5445 = CARTESIAN_POINT ( 'NONE',  ( 6.317381622560545473, 0.2407432673787524013, -0.1849999999999999978 ) ) ;
#5446 = CC_DESIGN_PERSON_AND_ORGANIZATION_ASSIGNMENT ( #154, #2697, ( #5925 ) ) ;
#5447 = DIRECTION ( 'NONE',  ( -0.2323175946639496336, 0.9726399823210830631, 0.000000000000000000 ) ) ;
#5448 = EDGE_CURVE ( 'NONE', #7766, #2842, #2319, .T. ) ;
#5449 = CARTESIAN_POINT ( 'NONE',  ( -0.03125000000000000000, 0.000000000000000000, 0.1106726592253027830 ) ) ;
#5450 = AXIS2_PLACEMENT_3D ( 'NONE', #5002, #5083, #6930 ) ;
#5451 = ORIENTED_EDGE ( 'NONE', *, *, #1569, .F. ) ;
#5452 = DIRECTION ( 'NONE',  ( 0.000000000000000000, 0.000000000000000000, 1.000000000000000000 ) ) ;
#5453 = AXIS2_PLACEMENT_3D ( 'NONE', #1304, #153, #3364 ) ;
#5454 = AXIS2_PLACEMENT_3D ( 'NONE', #2058, #4471, #6974 ) ;
#5455 = DIRECTION ( 'NONE',  ( -0.000000000000000000, -0.000000000000000000, 1.000000000000000000 ) ) ;
#5456 = DIRECTION ( 'NONE',  ( 0.9987955914953421388, 0.04906492035527377366, -0.000000000000000000 ) ) ;
#5457 = APPROVAL_STATUS ( 'not_yet_approved' ) ;
#5458 = ORIENTED_EDGE ( 'NONE', *, *, #7041, .T. ) ;
#5459 = DIRECTION ( 'NONE',  ( -0.000000000000000000, -1.000000000000000000, -0.000000000000000000 ) ) ;
#5460 = CIRCLE ( 'NONE', #7810, 0.3547681700190749576 ) ;
#5461 = FACE_OUTER_BOUND ( 'NONE', #7352, .T. ) ;
#5462 = PRODUCT_DEFINITION_SHAPE ( 'NONE', 'NONE',  #5651 ) ;
#5463 = FACE_OUTER_BOUND ( 'NONE', #2208, .T. ) ;
#5464 = CIRCLE ( 'NONE', #1268, 9.004497838701041701 ) ;
#5465 = ORIENTED_EDGE ( 'NONE', *, *, #7439, .F. ) ;
#5466 = AXIS2_PLACEMENT_3D ( 'NONE', #4307, #8017, #7421 ) ;
#5467 = ORIENTED_EDGE ( 'NONE', *, *, #1479, .T. ) ;
#5468 = FACE_OUTER_BOUND ( 'NONE', #5763, .T. ) ;
#5469 = CARTESIAN_POINT ( 'NONE',  ( 0.1015201953414744812, -0.4584396209566467539, 0.2207432131843653500 ) ) ;
#5470 = ITEM_DEFINED_TRANSFORMATION ( 'NONE', 'NONE', #1460,  #3555 ) ;
#5471 = CARTESIAN_POINT ( 'NONE',  ( 1.339249842318065653, 1.071711091725345621, -0.1040000000000607383 ) ) ;
#5472 = VERTEX_POINT ( 'NONE', #2307 ) ;
#5473 = ORIENTED_EDGE ( 'NONE', *, *, #2989, .T. ) ;
#5474 = DIRECTION ( 'NONE',  ( -1.000000000000000000, 0.000000000000000000, 0.000000000000000000 ) ) ;
#5475 = CARTESIAN_POINT ( 'NONE',  ( 0.08203198930727191585, -0.4609712184472686824, 0.02019114796704784762 ) ) ;
#5476 = CALENDAR_DATE ( 2026, 9, 10 ) ;
#5477 = CYLINDRICAL_SURFACE ( 'NONE', #3493, 9.064497838702109789 ) ;
#5478 = DIRECTION ( 'NONE',  ( -0.6568496200222107007, -0.7540216022612862279, 0.000000000000000000 ) ) ;
#5479 = ORIENTED_EDGE ( 'NONE', *, *, #6348, .T. ) ;
#5480 = LINE ( 'NONE', #2395, #5928 ) ;
#5481 = CARTESIAN_POINT ( 'NONE',  ( -0.09999999999999997780, -0.03125000000000000000, 0.06250000000000000000 ) ) ;
#5482 = VERTEX_POINT ( 'NONE', #300 ) ;
#5483 = ORIENTED_EDGE ( 'NONE', *, *, #133, .F. ) ;
#5484 = CARTESIAN_POINT ( 'NONE',  ( 0.000000000000000000, 0.000000000000000000, -0.6219999999999999973 ) ) ;
#5485 = CARTESIAN_POINT ( 'NONE',  ( -0.03125000000000000000, -0.03125000000000000000, 0.1162848326531996102 ) ) ;
#5486 = ADVANCED_FACE ( 'NONE', ( #1008 ), #2755, .T. ) ;
#5487 = EDGE_CURVE ( 'NONE', #5976, #6170, #6658, .T. ) ;
#5488 = EDGE_CURVE ( 'NONE', #5193, #4706, #3505, .T. ) ;
#5489 = CARTESIAN_POINT ( 'NONE',  ( -0.9280291358773672394, 0.8548654847802351631, -0.09374999999999998612 ) ) ;
#5490 = ORIENTED_EDGE ( 'NONE', *, *, #1080, .F. ) ;
#5491 = ORIENTED_EDGE ( 'NONE', *, *, #8081, .T. ) ;
#5492 = CARTESIAN_POINT ( 'NONE',  ( 1.680017506572348163, 1.266475429936566144, 0.1957466405106247642 ) ) ;
#5493 = CC_DESIGN_DATE_AND_TIME_ASSIGNMENT ( #1490, #4656, ( #3702 ) ) ;
#5494 = ADVANCED_FACE ( 'NONE', ( #4692 ), #2829, .T. ) ;
#5495 = CARTESIAN_POINT ( 'NONE',  ( 1.082008577329273136, 0.9412886604514951738, 0.03200000000000000067 ) ) ;
#5496 = DIRECTION ( 'NONE',  ( 0.2791259188691606608, 0.9602545086670756236, 0.000000000000000000 ) ) ;
#5497 = PERSON_AND_ORGANIZATION ( #4735, #6190 ) ;
#5498 = ORIENTED_EDGE ( 'NONE', *, *, #2801, .T. ) ;
#5499 = DIRECTION ( 'NONE',  ( -1.000000000000000000, 0.000000000000000000, 0.000000000000000000 ) ) ;
#5500 = CARTESIAN_POINT ( 'NONE',  ( 1.472069962421741263, 0.7095069109563477694, -0.1249999999999999306 ) ) ;
#5501 = ORIENTED_EDGE ( 'NONE', *, *, #6150, .T. ) ;
#5502 = CARTESIAN_POINT ( 'NONE',  ( 1.711017591405700422, 1.387320617706969461, 0.2054045915613178508 ) ) ;
#5503 = ORIENTED_EDGE ( 'NONE', *, *, #5086, .T. ) ;
#5504 =( NAMED_UNIT ( * ) PLANE_ANGLE_UNIT ( ) SI_UNIT ( $, .RADIAN. ) );
#5505 = ORIENTED_EDGE ( 'NONE', *, *, #7980, .F. ) ;
#5506 = DIRECTION ( 'NONE',  ( 0.000000000000000000, 0.000000000000000000, 1.000000000000000000 ) ) ;
#5507 = DATE_AND_TIME ( #4857, #5689 ) ;
#5508 = DIRECTION ( 'NONE',  ( -0.000000000000000000, 0.000000000000000000, 1.000000000000000000 ) ) ;
#5509 = ORIENTED_EDGE ( 'NONE', *, *, #6840, .T. ) ;
#5510 = ORIENTED_EDGE ( 'NONE', *, *, #3279, .T. ) ;
#5511 = CYLINDRICAL_SURFACE ( 'NONE', #2157, 0.2499962251234248700 ) ;
#5512 = DIRECTION ( 'NONE',  ( -0.7540216022612862279, 0.6568496200222109227, 0.000000000000000000 ) ) ;
#5513 = CARTESIAN_POINT ( 'NONE',  ( 0.7739487307887357170, -0.3852760516983189110, 0.07449999999999999678 ) ) ;
#5514 = PERSON_AND_ORGANIZATION ( #4735, #6190 ) ;
#5515 = CARTESIAN_POINT ( 'NONE',  ( 1.754394837573727051, 1.324599572866255848, 0.1638240367497202088 ) ) ;
#5516 = CARTESIAN_POINT ( 'NONE',  ( 1.647496491878244429, 1.712196251980273365, -0.06032347067126962725 ) ) ;
#5517 = ORIENTED_EDGE ( 'NONE', *, *, #2429, .F. ) ;
#5518 = CARTESIAN_POINT ( 'NONE',  ( 1.624003765053596116, 1.278431772831593261, 0.2011290015196109116 ) ) ;
#5519 = LINE ( 'NONE', #8007, #6069 ) ;
#5520 = LOCAL_TIME ( 14, 45, 32.00000000000000000, #2295 ) ;
#5521 = DIRECTION ( 'NONE',  ( -1.000000000000000000, 0.000000000000000000, 0.000000000000000000 ) ) ;
#5522 = CARTESIAN_POINT ( 'NONE',  ( 6.000000000000001776, 0.000000000000000000, 5.393636709996481038 ) ) ;
#5523 = SECURITY_CLASSIFICATION ( '', '', #4828 ) ;
#5524 = DIRECTION ( 'NONE',  ( 1.000000000000000000, 0.000000000000000000, 0.000000000000000000 ) ) ;
#5525 = ORIENTED_EDGE ( 'NONE', *, *, #1536, .T. ) ;
#5526 = FACE_OUTER_BOUND ( 'NONE', #4817, .T. ) ;
#5527 = VECTOR ( 'NONE', #3771, 39.37007874015748143 ) ;
#5528 = ADVANCED_FACE ( 'NONE', ( #1533 ), #4165, .F. ) ;
#5529 = CC_DESIGN_APPROVAL ( #2036, ( #3498 ) ) ;
#5530 = ADVANCED_FACE ( 'NONE', ( #7910 ), #4819, .T. ) ;
#5531 = CARTESIAN_POINT ( 'NONE',  ( 0.000000000000000000, 0.000000000000000000, 0.000000000000000000 ) ) ;
#5532 = DIRECTION ( 'NONE',  ( -0.000000000000000000, -0.000000000000000000, -1.000000000000000000 ) ) ;
#5533 = PERSON_AND_ORGANIZATION_ROLE ( 'design_owner' ) ;
#5534 = ORIENTED_EDGE ( 'NONE', *, *, #6191, .T. ) ;
#5535 = VECTOR ( 'NONE', #5958, 39.37007874015748143 ) ;
#5536 = CARTESIAN_POINT ( 'NONE',  ( 1.475891671935536609, 0.7226544316391472211, -0.09375000000000005551 ) ) ;
#5537 = EDGE_LOOP ( 'NONE', ( #3119, #4720 ) ) ;
#5538 = CARTESIAN_POINT ( 'NONE',  ( 1.803445950851875201, 1.337549153712537464, 0.2500000000004169443 ) ) ;
#5539 = EDGE_CURVE ( 'NONE', #5954, #6908, #7354, .T. ) ;
#5540 = EDGE_CURVE ( 'NONE', #1576, #3501, #803, .T. ) ;
#5541 = VECTOR ( 'NONE', #4088, 39.37007874015748143 ) ;
#5542 = ORIENTED_EDGE ( 'NONE', *, *, #2736, .T. ) ;
#5543 = EDGE_CURVE ( 'NONE', #4068, #91, #5342, .T. ) ;
#5544 = DIRECTION ( 'NONE',  ( -0.000000000000000000, 0.000000000000000000, 1.000000000000000000 ) ) ;
#5545 = LENGTH_MEASURE_WITH_UNIT ( LENGTH_MEASURE( 0.02539999999999999897 ), #6081 );
#5546 = CARTESIAN_POINT ( 'NONE',  ( -0.5950975756886834889, 0.1840126700235211188, 0.03200000000000000067 ) ) ;
#5547 = APPROVAL_DATE_TIME ( #7470, #7299 ) ;
#5548 = APPROVAL ( #2593, 'UNSPECIFIED' ) ;
#5549 = DIRECTION ( 'NONE',  ( 0.7879377495398138809, 0.6157549048526804736, 0.000000000000000000 ) ) ;
#5550 = EDGE_CURVE ( 'NONE', #2946, #4309, #5915, .T. ) ;
#5551 = VECTOR ( 'NONE', #4496, 39.37007874015748143 ) ;
#5552 = B_SPLINE_CURVE_WITH_KNOTS ( 'NONE', 3,
 ( #6700, #1087, #1128, #4976, #2973, #1740, #1821, #3136 ),
 .UNSPECIFIED., .F., .F.,
 ( 4, 2, 2, 4 ),
 ( 6.554322722250637004E-16, 0.001190714077523056602, 0.001786071116284258234, 0.002381428155045459648 ),
 .UNSPECIFIED. ) ;
#5553 = AXIS2_PLACEMENT_3D ( 'NONE', #2729, #3840, #722 ) ;
#5554 = ORIENTED_EDGE ( 'NONE', *, *, #426, .F. ) ;
#5555 = DIRECTION ( 'NONE',  ( 1.000000000000000000, 0.000000000000000000, 0.000000000000000000 ) ) ;
#5556 = CARTESIAN_POINT ( 'NONE',  ( 3.666415866878782737, -8.185094079965432812, 0.1250000000000000000 ) ) ;
#5557 = CARTESIAN_POINT ( 'NONE',  ( 0.09357815549526610210, -0.4595590400308178780, 0.02446392532630315905 ) ) ;
#5558 = MECHANICAL_CONTEXT ( 'NONE', #4207, 'mechanical' ) ;
#5559 = CARTESIAN_POINT ( 'NONE',  ( 1.877707900143042563, 1.420965844381539167, -0.06059890939898970180 ) ) ;
#5560 = LINE ( 'NONE', #6866, #2412 ) ;
#5561 = VERTEX_POINT ( 'NONE', #7182 ) ;
#5562 = FACE_BOUND ( 'NONE', #4193, .T. ) ;
#5563 = LOCAL_TIME ( 14, 45, 32.00000000000000000, #2968 ) ;
#5564 = AXIS2_PLACEMENT_3D ( 'NONE', #6135, #2348, #5638 ) ;
#5565 = B_SPLINE_CURVE_WITH_KNOTS ( 'NONE', 3,
 ( #2228, #4723, #1609, #4114, #380, #7865, #4770, #6657 ),
 .UNSPECIFIED., .F., .F.,
 ( 4, 2, 2, 4 ),
 ( 0.0003409113597368014937, 0.001278283151453492609, 0.001746969047311835348, 0.002215654943170178304 ),
 .UNSPECIFIED. ) ;
#5566 = VECTOR ( 'NONE', #3678, 39.37007874015748143 ) ;
#5567 = ORIENTED_EDGE ( 'NONE', *, *, #6046, .F. ) ;
#5568 = CYLINDRICAL_SURFACE ( 'NONE', #6336, 0.4999999999999997224 ) ;
#5569 = CARTESIAN_POINT ( 'NONE',  ( 1.496213642433631197, 1.858935772646855611, -0.1039999999999998703 ) ) ;
#5570 = PLANE ( 'NONE',  #6365 ) ;
#5571 = VERTEX_POINT ( 'NONE', #368 ) ;
#5572 = ORIENTED_EDGE ( 'NONE', *, *, #4054, .F. ) ;
#5573 = CARTESIAN_POINT ( 'NONE',  ( 0.07000000000000002054, 0.03125000000000000000, 0.8125000000000000000 ) ) ;
#5574 = APPLICATION_CONTEXT ( 'configuration controlled 3d designs of mechanical parts and assemblies' ) ;
#5575 = CIRCLE ( 'NONE', #5708, 0.09374999999999998612 ) ;
#5576 = CARTESIAN_POINT ( 'NONE',  ( 1.731490805948541212, 1.384744806418967356, 0.1971537411642678150 ) ) ;
#5577 = DIRECTION ( 'NONE',  ( 0.000000000000000000, 0.000000000000000000, -1.000000000000000000 ) ) ;
#5578 = AXIS2_PLACEMENT_3D ( 'NONE', #3211, #6976, #5174 ) ;
#5579 = PERSON_AND_ORGANIZATION ( #4735, #6190 ) ;
#5580 = ORIENTED_EDGE ( 'NONE', *, *, #6552, .F. ) ;
#5581 = DIRECTION ( 'NONE',  ( 0.7879377495398141029, 0.6157549048526802515, 0.000000000000000000 ) ) ;
#5582 = DIRECTION ( 'NONE',  ( -0.6157549048526803626, 0.7879377495398141029, -0.000000000000000000 ) ) ;
#5583 = EDGE_CURVE ( 'NONE', #4303, #5391, #3527, .T. ) ;
#5584 = VECTOR ( 'NONE', #4582, 39.37007874015748143 ) ;
#5585 = LINE ( 'NONE', #3700, #5933 ) ;
#5586 = CIRCLE ( 'NONE', #3755, 0.2499962251234248700 ) ;
#5587 = ORIENTED_EDGE ( 'NONE', *, *, #732, .T. ) ;
#5588 = AXIS2_PLACEMENT_3D ( 'NONE', #4871, #8049, #6063 ) ;
#5589 = CIRCLE ( 'NONE', #3362, 0.1799999999999999933 ) ;
#5590 = CARTESIAN_POINT ( 'NONE',  ( 1.800863856793468276, 1.423917841411510343, 0.1209648279927613007 ) ) ;
#5591 = DIRECTION ( 'NONE',  ( 0.7879377495398222075, 0.6157549048526698154, 0.000000000000000000 ) ) ;
#5592 = COORDINATED_UNIVERSAL_TIME_OFFSET ( 0, 0, .AHEAD. ) ;
#5593 = EDGE_CURVE ( 'NONE', #3711, #5193, #4033, .T. ) ;
#5594 = PLANE ( 'NONE',  #5443 ) ;
#5595 = EDGE_CURVE ( 'NONE', #7842, #3419, #5377, .T. ) ;
#5596 = ADVANCED_FACE ( 'NONE', ( #7823 ), #2218, .T. ) ;
#5597 = AXIS2_PLACEMENT_3D ( 'NONE', #498, #1, #659 ) ;
#5598 = APPROVAL ( #6331, 'UNSPECIFIED' ) ;
#5599 = ADVANCED_FACE ( 'NONE', ( #7898 ), #1454, .T. ) ;
#5600 = ORIENTED_EDGE ( 'NONE', *, *, #728, .T. ) ;
#5601 = EDGE_LOOP ( 'NONE', ( #717, #6259, #7044, #5580, #5302 ) ) ;
#5602 = EDGE_CURVE ( 'NONE', #796, #4126, #4103, .T. ) ;
#5603 = DIRECTION ( 'NONE',  ( -0.000000000000000000, -0.000000000000000000, -1.000000000000000000 ) ) ;
#5604 = FACE_OUTER_BOUND ( 'NONE', #5278, .T. ) ;
#5606 = FACE_OUTER_BOUND ( 'NONE', #6507, .T. ) ;
#5605 = CIRCLE ( 'NONE', #4164, 0.03200000000000007699 ) ;
#5607 = DATE_AND_TIME ( #5018, #3439 ) ;
#5608 = DIRECTION ( 'NONE',  ( -1.000000000000000000, -7.137164547826461966E-15, 0.000000000000000000 ) ) ;
#5609 = CIRCLE ( 'NONE', #2706, 8.696493751522730520 ) ;
#5610 = CARTESIAN_POINT ( 'NONE',  ( 1.597024068692529220, 1.785137331457983700, -2.037143834727303156E-14 ) ) ;
#5611 = ORIENTED_EDGE ( 'NONE', *, *, #4042, .F. ) ;
#5612 = DIRECTION ( 'NONE',  ( -0.000000000000000000, 0.000000000000000000, -1.000000000000000000 ) ) ;
#5613 = ORIENTED_EDGE ( 'NONE', *, *, #4589, .T. ) ;
#5614 = LINE ( 'NONE', #2481, #6468 ) ;
#5615 = CARTESIAN_POINT ( 'NONE',  ( 1.271405812440770999, 1.084215362033057017, -0.08402758940906858431 ) ) ;
#5616 = CARTESIAN_POINT ( 'NONE',  ( -0.03125000000000000000, -0.03125000000000000000, -0.1162848326531996102 ) ) ;
#5617 = EDGE_LOOP ( 'NONE', ( #240, #8037 ) ) ;
#5618 = ORIENTED_EDGE ( 'NONE', *, *, #3685, .F. ) ;
#5619 = DIRECTION ( 'NONE',  ( 0.000000000000000000, 1.000000000000000000, 0.000000000000000000 ) ) ;
#5620 = DIRECTION ( 'NONE',  ( 0.7540216022612862279, -0.6568496200222107007, 0.000000000000000000 ) ) ;
#5621 = DIRECTION ( 'NONE',  ( 0.000000000000000000, -1.000000000000000000, 0.000000000000000000 ) ) ;
#5622 = APPROVAL_ROLE ( '' ) ;
#5623 = ORIENTED_EDGE ( 'NONE', *, *, #5543, .F. ) ;
#5624 = LINE ( 'NONE', #1889, #227 ) ;
#5625 = CARTESIAN_POINT ( 'NONE',  ( -1.194903880989551359, -0.2358655892081394090, 0.2500000000000000000 ) ) ;
#5626 = ORIENTED_EDGE ( 'NONE', *, *, #5043, .T. ) ;
#5627 = CARTESIAN_POINT ( 'NONE',  ( 3.672798492683009286, -8.252032378159654513, 0.1250000000000004441 ) ) ;
#5628 = ORIENTED_EDGE ( 'NONE', *, *, #5794, .F. ) ;
#5629 = CARTESIAN_POINT ( 'NONE',  ( 1.788798563727062474, 1.414764706470791333, 0.1365599753587105336 ) ) ;
#5630 = CARTESIAN_POINT ( 'NONE',  ( 0.000000000000000000, 1.362500000000000044, 0.000000000000000000 ) ) ;
#5631 = DIMENSIONAL_EXPONENTS ( 1.000000000000000000, 0.000000000000000000, 0.000000000000000000, 0.000000000000000000, 0.000000000000000000, 0.000000000000000000, 0.000000000000000000 ) ;
#5632 = SECURITY_CLASSIFICATION_LEVEL ( 'unclassified' ) ;
#5633 = LINE ( 'NONE', #4937, #997 ) ;
#5634 = EDGE_CURVE ( 'NONE', #762, #5236, #2582, .T. ) ;
#5635 = EDGE_CURVE ( 'NONE', #1079, #5277, #3901, .T. ) ;
#5636 = ADVANCED_FACE ( 'NONE', ( #4034 ), #3447, .F. ) ;
#5637 = ORIENTED_EDGE ( 'NONE', *, *, #2781, .F. ) ;
#5638 = DIRECTION ( 'NONE',  ( -0.7879377495398141029, -0.6157549048526801405, 0.000000000000000000 ) ) ;
#5639 = DIRECTION ( 'NONE',  ( 0.000000000000000000, -1.000000000000000000, 0.000000000000000000 ) ) ;
#5640 = CARTESIAN_POINT ( 'NONE',  ( -0.01466378298870799936, -0.4621478854113529322, 0.0009103679542912866511 ) ) ;
#5641 = APPROVAL_ROLE ( '' ) ;
#5642 = CARTESIAN_POINT ( 'NONE',  ( -0.1875000000000000278, 0.000000000000000000, 0.1250000000000000000 ) ) ;
#5643 = CARTESIAN_POINT ( 'NONE',  ( 1.762538566111710558, 1.560058259527964619, -0.03170243290436908223 ) ) ;
#5644 = ORIENTED_EDGE ( 'NONE', *, *, #4887, .F. ) ;
#5645 = CC_DESIGN_DATE_AND_TIME_ASSIGNMENT ( #6486, #921, ( #5404 ) ) ;
#5646 = EDGE_CURVE ( 'NONE', #963, #8047, #6535, .T. ) ;
#5647 = ADVANCED_FACE ( 'NONE', ( #1188 ), #6884, .F. ) ;
#5648 = ORIENTED_EDGE ( 'NONE', *, *, #7629, .F. ) ;
#5649 = DIRECTION ( 'NONE',  ( -0.6568496200222107007, -0.7540216022612862279, 0.000000000000000000 ) ) ;
#5650 = DIRECTION ( 'NONE',  ( -0.000000000000000000, -1.000000000000000000, -0.000000000000000000 ) ) ;
#5651 = PRODUCT_DEFINITION ( 'UNKNOWN', '', #4480, #1549 ) ;
#5652 = CARTESIAN_POINT ( 'NONE',  ( 0.02822771919327313195, 0.03615965030275954117, 0.2500000000000000000 ) ) ;
#5653 = ADVANCED_FACE ( 'NONE', ( #7977 ), #495, .T. ) ;
#5654 = EDGE_LOOP ( 'NONE', ( #2071, #4458, #459, #3671 ) ) ;
#5655 = CARTESIAN_POINT ( 'NONE',  ( 1.087752123103788326, 1.539732657782964864, -0.2121970708454803678 ) ) ;
#5656 = ORIENTED_EDGE ( 'NONE', *, *, #2383, .F. ) ;
#5657 = DIRECTION ( 'NONE',  ( -0.6157549048526802515, 0.7879377495398142139, -0.000000000000000000 ) ) ;
#5658 = APPROVAL_PERSON_ORGANIZATION ( #6282, #3146, #5622 ) ;
#5659 = CARTESIAN_POINT ( 'NONE',  ( 1.584990804742211212, 1.283332362320874998, 0.2375404096856918168 ) ) ;
#5660 = APPLICATION_PROTOCOL_DEFINITION ( 'international standard', 'config_control_design', 1994, #2518 ) ;
#5661 = ORIENTED_EDGE ( 'NONE', *, *, #270, .F. ) ;
#5662 = CARTESIAN_POINT ( 'NONE',  ( 1.345710376364902983, 1.085941737115722283, -0.1453092053285080509 ) ) ;
#5663 = FACE_OUTER_BOUND ( 'NONE', #5774, .T. ) ;
#5664 = TOROIDAL_SURFACE ( 'NONE', #4356, 0.1487499999999999933, 0.03125000000000000000 ) ;
#5665 = CARTESIAN_POINT ( 'NONE',  ( -1.411633252941551397, 0.8434166392007489410, -0.09374999999999998612 ) ) ;
#5666 = SECURITY_CLASSIFICATION ( '', '', #5097 ) ;
#5667 = AXIS2_PLACEMENT_3D ( 'NONE', #1389, #6288, #5747 ) ;
#5668 = DIRECTION ( 'NONE',  ( 0.6157549048526801405, -0.7879377495398139919, 0.000000000000000000 ) ) ;
#5669 = DIRECTION ( 'NONE',  ( 0.000000000000000000, 0.000000000000000000, 1.000000000000000000 ) ) ;
#5670 = CARTESIAN_POINT ( 'NONE',  ( 0.000000000000000000, 0.000000000000000000, -0.6849999999999999423 ) ) ;
#5671 = LOCAL_TIME ( 14, 45, 32.00000000000000000, #629 ) ;
#5672 = PERSON_AND_ORGANIZATION ( #6518, #5305 ) ;
#5673 = CARTESIAN_POINT ( 'NONE',  ( -1.411841654243101596, 0.8435981834898315102, -0.1250000000000000000 ) ) ;
#5674 = VECTOR ( 'NONE', #5294, 39.37007874015748143 ) ;
#5675 = ORIENTED_EDGE ( 'NONE', *, *, #1546, .T. ) ;
#5676 = VERTEX_POINT ( 'NONE', #566 ) ;
#5677 = CARTESIAN_POINT ( 'NONE',  ( 0.000000000000000000, 0.000000000000000000, -0.6229999999999998872 ) ) ;
#5678 = CIRCLE ( 'NONE', #2526, 0.4060000000000001386 ) ;
#5679 = FACE_OUTER_BOUND ( 'NONE', #2959, .T. ) ;
#5680 = PERSON_AND_ORGANIZATION ( #4735, #6190 ) ;
#5681 = CARTESIAN_POINT ( 'NONE',  ( -1.023858060246952029, -0.8104042351526981047, -0.05999999999999999778 ) ) ;
#5682 = PLANE ( 'NONE',  #1634 ) ;
#5683 = AXIS2_PLACEMENT_3D ( 'NONE', #4325, #6137, #1131 ) ;
#5684 = AXIS2_PLACEMENT_3D ( 'NONE', #3009, #5506, #7991 ) ;
#5685 = DIRECTION ( 'NONE',  ( -1.000000000000000000, 0.000000000000000000, 0.000000000000000000 ) ) ;
#5686 = VERTEX_POINT ( 'NONE', #3156 ) ;
#5687 = CARTESIAN_POINT ( 'NONE',  ( 0.000000000000000000, 0.03125000000000000000, 0.000000000000000000 ) ) ;
#5688 = CARTESIAN_POINT ( 'NONE',  ( -0.1250000000000000000, 0.5625000000000000000, -0.03125000000000000000 ) ) ;
#5689 = LOCAL_TIME ( 14, 45, 32.00000000000000000, #3132 ) ;
#5690 = VECTOR ( 'NONE', #3374, 39.37007874015748143 ) ;
#5691 = CARTESIAN_POINT ( 'NONE',  ( 1.738285998806500032, 1.406929468094443969, 0.1853310783740557410 ) ) ;
#5692 = EDGE_CURVE ( 'NONE', #3041, #1125, #3511, .T. ) ;
#5693 = ORIENTED_EDGE ( 'NONE', *, *, #4403, .T. ) ;
#5694 = EDGE_CURVE ( 'NONE', #3319, #3658, #8070, .T. ) ;
#5695 = PLANE ( 'NONE',  #6591 ) ;
#5696 = EDGE_CURVE ( 'NONE', #2220, #6326, #3072, .T. ) ;
#5697 = AXIS2_PLACEMENT_3D ( 'NONE', #5136, #139, #2595 ) ;
#5698 = TOROIDAL_SURFACE ( 'NONE', #1635, 0.4070000000000000839, 0.03200000000000000067 ) ;
#5699 = APPROVAL ( #7316, 'UNKNOWN' ) ;
#5700 = ADVANCED_FACE ( 'NONE', ( #6842 ), #3777, .F. ) ;
#5701 = EDGE_LOOP ( 'NONE', ( #1812, #3345, #4741, #6612 ) ) ;
#5702 = DIRECTION ( 'NONE',  ( 0.000000000000000000, 0.000000000000000000, -1.000000000000000000 ) ) ;
#5703 = FACE_OUTER_BOUND ( 'NONE', #5303, .T. ) ;
#5704 = CALENDAR_DATE ( 2026, 9, 10 ) ;
#5705 = ORIENTED_EDGE ( 'NONE', *, *, #4695, .T. ) ;
#5706 = DIRECTION ( 'NONE',  ( -1.000000000000000000, 0.000000000000000000, 0.000000000000000000 ) ) ;
#5707 = CARTESIAN_POINT ( 'NONE',  ( 1.723350842796532278, 1.129006085766179890, -0.1039999999999998703 ) ) ;
#5708 = AXIS2_PLACEMENT_3D ( 'NONE', #7350, #7993, #6695 ) ;
#5709 = CARTESIAN_POINT ( 'NONE',  ( -1.763177565995707630, 1.070083551578369763, 0.1339999999999995361 ) ) ;
#5710 = AXIS2_PLACEMENT_3D ( 'NONE', #5346, #1565, #7262 ) ;
#5711 = CARTESIAN_POINT ( 'NONE',  ( 0.9690125299525021996, 0.8529848947786565772, 0.2179999999999999993 ) ) ;
#5712 = APPROVAL_STATUS ( 'not_yet_approved' ) ;
#5713 = CARTESIAN_POINT ( 'NONE',  ( 1.411244833761398310, 1.056435878372752324, -0.1949596646313069837 ) ) ;
#5714 = DIRECTION ( 'NONE',  ( 0.000000000000000000, 0.000000000000000000, 1.000000000000000000 ) ) ;
#5715 = VECTOR ( 'NONE', #3606, 39.37007874015748143 ) ;
#5716 = VERTEX_POINT ( 'NONE', #2365 ) ;
#5717 = VECTOR ( 'NONE', #7890, 39.37007874015748143 ) ;
#5718 = CIRCLE ( 'NONE', #2441, 0.03125000000000000000 ) ;
#5719 = ORIENTED_EDGE ( 'NONE', *, *, #11, .T. ) ;
#5720 = CARTESIAN_POINT ( 'NONE',  ( 0.000000000000000000, 0.000000000000000000, 0.000000000000000000 ) ) ;
#5721 = ORIENTED_EDGE ( 'NONE', *, *, #6181, .F. ) ;
#5722 = CARTESIAN_POINT ( 'NONE',  ( 1.420352459187311345, 1.205696483155414001, 0.2500000000000000000 ) ) ;
#5723 = PERSON_AND_ORGANIZATION_ROLE ( 'design_supplier' ) ;
#5724 = CARTESIAN_POINT ( 'NONE',  ( 1.764573863409885313, 1.564560119641652092, -0.07057956653668050195 ) ) ;
#5725 = DIRECTION ( 'NONE',  ( 1.000000000000000000, 0.000000000000000000, 0.000000000000000000 ) ) ;
#5726 = ORIENTED_EDGE ( 'NONE', *, *, #6979, .T. ) ;
#5727 = CIRCLE ( 'NONE', #1392, 6.870657474112407570 ) ;
#5728 = CIRCLE ( 'NONE', #4158, 9.004497838701041701 ) ;
#5729 = AXIS2_PLACEMENT_3D ( 'NONE', #7379, #1764, #4966 ) ;
#5730 = ORIENTED_EDGE ( 'NONE', *, *, #6393, .F. ) ;
#5731 = AXIS2_PLACEMENT_3D ( 'NONE', #6281, #656, #6158 ) ;
#5732 = DIRECTION ( 'NONE',  ( -0.5901435170775125583, 0.000000000000000000, -0.8072983520677988745 ) ) ;
#5733 = ORIENTED_EDGE ( 'NONE', *, *, #5583, .T. ) ;
#5734 = FACE_OUTER_BOUND ( 'NONE', #2633, .T. ) ;
#5735 = CARTESIAN_POINT ( 'NONE',  ( 1.403524466810122107, 1.061529367020492831, -0.1913948864930017091 ) ) ;
#5736 = CARTESIAN_POINT ( 'NONE',  ( -1.411633252941551619, 0.8434166392007494961, 0.09374999999999998612 ) ) ;
#5737 = DIRECTION ( 'NONE',  ( -0.7879377495398141029, -0.6157549048526801405, 0.000000000000000000 ) ) ;
#5738 = EDGE_CURVE ( 'NONE', #6563, #2698, #8058, .T. ) ;
#5739 = EDGE_CURVE ( 'NONE', #4364, #3462, #5218, .T. ) ;
#5740 = CARTESIAN_POINT ( 'NONE',  ( 1.823361563706781707, 1.441291881570038402, 0.08644244353395109937 ) ) ;
#5741 = CARTESIAN_POINT ( 'NONE',  ( -1.543211452806561912, 0.6927940070358482583, 0.1250000000000000000 ) ) ;
#5742 = CALENDAR_DATE ( 2026, 9, 10 ) ;
#5743 = ORIENTED_EDGE ( 'NONE', *, *, #1085, .F. ) ;
#5744 = CARTESIAN_POINT ( 'NONE',  ( 1.512219939927767820, 1.830831974065061596, -0.05383208248537842133 ) ) ;
#5745 = CARTESIAN_POINT ( 'NONE',  ( 3.666415866878782737, -8.185094079965432812, 0.1849999999999999978 ) ) ;
#5746 = ORIENTED_EDGE ( 'NONE', *, *, #2084, .T. ) ;
#5747 = DIRECTION ( 'NONE',  ( 1.000000000000000000, 1.417505363144159755E-14, 0.000000000000000000 ) ) ;
#5748 = CARTESIAN_POINT ( 'NONE',  ( -0.5950975756886835999, 0.1840126700235212853, 0.2500000000000000000 ) ) ;
#5749 = DIRECTION ( 'NONE',  ( 0.7540216022612868940, -0.6568496200222100345, -3.330669073875469621E-16 ) ) ;
#5750 = CARTESIAN_POINT ( 'NONE',  ( 0.2976660692273699338, -0.3850326757561698954, 0.000000000000000000 ) ) ;
#5751 = CALENDAR_DATE ( 2026, 9, 10 ) ;
#5752 = CARTESIAN_POINT ( 'NONE',  ( 1.723083782080649939, 1.395997476760423961, 0.1965221205739769994 ) ) ;
#5753 = PLANE ( 'NONE',  #4478 ) ;
#5754 = ORIENTED_EDGE ( 'NONE', *, *, #5543, .T. ) ;
#5755 = ORIENTED_EDGE ( 'NONE', *, *, #2383, .T. ) ;
#5756 = EDGE_LOOP ( 'NONE', ( #6387, #7616, #7859, #1712 ) ) ;
#5757 = CARTESIAN_POINT ( 'NONE',  ( 0.1250000000000000278, -0.03125000000000000000, 0.06250000000000000000 ) ) ;
#5758 = DIRECTION ( 'NONE',  ( 0.000000000000000000, -1.000000000000000000, 0.000000000000000000 ) ) ;
#5759 = PERSON_AND_ORGANIZATION_ROLE ( 'classification_officer' ) ;
#5760 = CARTESIAN_POINT ( 'NONE',  ( -0.04782642554762441683, -0.03125000000000000000, 0.000000000000000000 ) ) ;
#5761 = LINE ( 'NONE', #7067, #7913 ) ;
#5762 = ORIENTED_EDGE ( 'NONE', *, *, #7827, .F. ) ;
#5763 = EDGE_LOOP ( 'NONE', ( #5805, #1483 ) ) ;
#5764 = DIRECTION ( 'NONE',  ( -0.9968059542140785823, 0.000000000000000000, 0.07986169071188248259 ) ) ;
#5765 = ORIENTED_EDGE ( 'NONE', *, *, #3887, .T. ) ;
#5766 = CARTESIAN_POINT ( 'NONE',  ( 1.662633195254459739, 1.344068888399850392, 0.2328741875126813521 ) ) ;
#5767 = DIRECTION ( 'NONE',  ( 1.000000000000000000, 0.000000000000000000, 0.000000000000000000 ) ) ;
#5768 = LINE ( 'NONE', #7488, #6968 ) ;
#5769 = FACE_OUTER_BOUND ( 'NONE', #7416, .T. ) ;
#5770 = ORIENTED_EDGE ( 'NONE', *, *, #2791, .F. ) ;
#5771 = CARTESIAN_POINT ( 'NONE',  ( 1.801196254061721680, 1.424171435408524644, 0.1205097783069856016 ) ) ;
#5772 = DIRECTION ( 'NONE',  ( 1.000000000000000000, 0.000000000000000000, 0.000000000000000000 ) ) ;
#5773 = APPROVAL_STATUS ( 'not_yet_approved' ) ;
#5774 = EDGE_LOOP ( 'NONE', ( #2469, #3129, #7751, #2305, #6133, #99, #6004, #2199 ) ) ;
#5775 = DIRECTION ( 'NONE',  ( 1.000000000000000000, 0.000000000000000000, 0.000000000000000000 ) ) ;
#5776 = CYLINDRICAL_SURFACE ( 'NONE', #5450, 0.2500000000000000555 ) ;
#5777 = ORIENTED_EDGE ( 'NONE', *, *, #5945, .F. ) ;
#5778 = CARTESIAN_POINT ( 'NONE',  ( 0.1250000000000000000, 0.6250000000000000000, -0.03125000000000000000 ) ) ;
#5779 = CARTESIAN_POINT ( 'NONE',  ( 0.000000000000000000, 0.6124999999999999334, 0.000000000000000000 ) ) ;
#5780 = DIRECTION ( 'NONE',  ( 0.000000000000000000, 0.000000000000000000, 1.000000000000000000 ) ) ;
#5781 = CARTESIAN_POINT ( 'NONE',  ( -1.420319797626316438, 0.8334728170008731674, -0.1249999999999997641 ) ) ;
#5782 = DIRECTION ( 'NONE',  ( 0.000000000000000000, 0.000000000000000000, 1.000000000000000000 ) ) ;
#5783 =( GEOMETRIC_REPRESENTATION_CONTEXT ( 3 ) GLOBAL_UNCERTAINTY_ASSIGNED_CONTEXT ( ( #390 ) ) GLOBAL_UNIT_ASSIGNED_CONTEXT ( ( #5132, #4451, #6946 ) ) REPRESENTATION_CONTEXT ( 'NONE', 'WORKASPACE' ) );
#5784 = DIRECTION ( 'NONE',  ( 0.000000000000000000, 0.000000000000000000, -1.000000000000000000 ) ) ;
#5785 = CC_DESIGN_APPROVAL ( #2739, ( #5925 ) ) ;
#5786 = CC_DESIGN_SECURITY_CLASSIFICATION ( #3702, ( #8093 ) ) ;
#5787 = EDGE_CURVE ( 'NONE', #1684, #1575, #7303, .T. ) ;
#5788 = EDGE_CURVE ( 'NONE', #8047, #1448, #5609, .T. ) ;
#5789 = EDGE_CURVE ( 'NONE', #5139, #3273, #2064, .T. ) ;
#5790 = AXIS2_PLACEMENT_3D ( 'NONE', #312, #2820, #7813 ) ;
#5791 = AXIS2_PLACEMENT_3D ( 'NONE', #3743, #5749, #1966 ) ;
#5792 = LOCAL_TIME ( 14, 45, 32.00000000000000000, #2718 ) ;
#5793 = CC_DESIGN_PERSON_AND_ORGANIZATION_ASSIGNMENT ( #5042, #3855, ( #3600 ) ) ;
#5794 = EDGE_CURVE ( 'NONE', #6217, #6544, #896, .T. ) ;
#5795 = DIRECTION ( 'NONE',  ( -0.000000000000000000, 0.000000000000000000, 1.000000000000000000 ) ) ;
#5796 = CARTESIAN_POINT ( 'NONE',  ( 0.1250000000000000000, 1.530808498934191509E-17, -0.1250000000000000000 ) ) ;
#5797 = ADVANCED_FACE ( 'NONE', ( #2489 ), #6767, .F. ) ;
#5798 = CALENDAR_DATE ( 2026, 9, 10 ) ;
#5799 = DIRECTION ( 'NONE',  ( 0.000000000000000000, 0.000000000000000000, 1.000000000000000000 ) ) ;
#5800 = DIRECTION ( 'NONE',  ( 0.000000000000000000, 0.000000000000000000, 1.000000000000000000 ) ) ;
#5801 = B_SPLINE_CURVE_WITH_KNOTS ( 'NONE', 3,
 ( #5091, #1351, #7671, #3823, #6324, #130, #7019, #1283 ),
 .UNSPECIFIED., .F., .F.,
 ( 4, 2, 2, 4 ),
 ( -7.741103271180475610E-06, 0.0006266493673793644076, 0.0009438446027046368475, 0.001261039838029909179 ),
 .UNSPECIFIED. ) ;
#5802 = AXIS2_PLACEMENT_3D ( 'NONE', #6433, #87, #122 ) ;
#5803 = VERTEX_POINT ( 'NONE', #1151 ) ;
#5804 = CIRCLE ( 'NONE', #7110, 0.2499400561648078278 ) ;
#5805 = ORIENTED_EDGE ( 'NONE', *, *, #7588, .T. ) ;
#5806 = CARTESIAN_POINT ( 'NONE',  ( 1.800320205903116921, 1.030513867073702183, -0.08212881570848259982 ) ) ;
#5807 = EDGE_LOOP ( 'NONE', ( #5890, #4421, #134, #207 ) ) ;
#5808 = CARTESIAN_POINT ( 'NONE',  ( -1.763177565995707630, 1.070083551578369763, -0.2959999999999997078 ) ) ;
#5809 = CARTESIAN_POINT ( 'NONE',  ( -0.1210307295689817542, 0.6124999999999999334, -0.03125000000000000000 ) ) ;
#5810 = DIRECTION ( 'NONE',  ( 0.000000000000000000, 0.000000000000000000, 1.000000000000000000 ) ) ;
#5811 = AXIS2_PLACEMENT_3D ( 'NONE', #7126, #1507, #4019 ) ;
#5812 = DIRECTION ( 'NONE',  ( 0.000000000000000000, 0.000000000000000000, 1.000000000000000000 ) ) ;
#5813 = CIRCLE ( 'NONE', #575, 6.870657474112407570 ) ;
#5814 = CARTESIAN_POINT ( 'NONE',  ( 1.473794063193210269, 1.841415396333994314, 0.05205027013366145955 ) ) ;
#5815 = LINE ( 'NONE', #7655, #3879 ) ;
#5816 = PERSON_AND_ORGANIZATION ( #4735, #6190 ) ;
#5817 = ORIENTED_EDGE ( 'NONE', *, *, #2621, .F. ) ;
#5818 = DIRECTION ( 'NONE',  ( -0.000000000000000000, -0.000000000000000000, -1.000000000000000000 ) ) ;
#5819 = CARTESIAN_POINT ( 'NONE',  ( 0.3095776802284428975, -0.3772299648020716600, 0.0005848437636013204509 ) ) ;
#5820 = ORIENTED_EDGE ( 'NONE', *, *, #6807, .T. ) ;
#5821 = DIRECTION ( 'NONE',  ( 1.000000000000000000, 0.000000000000000000, -0.000000000000000000 ) ) ;
#5822 = CC_DESIGN_APPROVAL ( #1233, ( #1357 ) ) ;
#5823 = CARTESIAN_POINT ( 'NONE',  ( 0.03125000000000000000, 0.7500000000000001110, -0.1106726592253027691 ) ) ;
#5824 = CARTESIAN_POINT ( 'NONE',  ( 0.6690408158126811555, -0.04637372973215107830, 0.000000000000000000 ) ) ;
#5825 = VECTOR ( 'NONE', #7721, 39.37007874015748143 ) ;
#5826 = APPROVAL_ROLE ( '' ) ;
#5827 = ADVANCED_FACE ( 'NONE', ( #4997 ), #4393, .T. ) ;
#5828 = ORIENTED_EDGE ( 'NONE', *, *, #5602, .F. ) ;
#5829 = CIRCLE ( 'NONE', #8036, 0.03200000000000002148 ) ;
#5830 = VERTEX_POINT ( 'NONE', #1807 ) ;
#5831 = CARTESIAN_POINT ( 'NONE',  ( 1.877688265130482037, 1.420950500079102286, -0.07807135826935437950 ) ) ;
#5832 = DIRECTION ( 'NONE',  ( -1.000000000000000000, 1.224646799147352714E-16, 0.000000000000000000 ) ) ;
#5833 = ORIENTED_EDGE ( 'NONE', *, *, #7459, .T. ) ;
#5834 = CIRCLE ( 'NONE', #864, 0.1250000000000000000 ) ;
#5835 = ORIENTED_EDGE ( 'NONE', *, *, #1275, .F. ) ;
#5836 = ORIENTED_EDGE ( 'NONE', *, *, #4403, .F. ) ;
#5837 = EDGE_CURVE ( 'NONE', #4081, #3263, #1149, .T. ) ;
#5838 = EDGE_CURVE ( 'NONE', #5927, #2759, #1340, .T. ) ;
#5839 = EDGE_CURVE ( 'NONE', #2344, #3415, #602, .T. ) ;
#5840 = DIRECTION ( 'NONE',  ( 0.6157549048526804736, -0.7879377495398138809, 0.000000000000000000 ) ) ;
#5841 = DATE_AND_TIME ( #3949, #7754 ) ;
#5842 = DIRECTION ( 'NONE',  ( -0.6157549048526802515, 0.7879377495398141029, -0.000000000000000000 ) ) ;
#5843 = DIRECTION ( 'NONE',  ( 0.6157549048526803626, -0.7879377495398141029, 0.000000000000000000 ) ) ;
#5845 = VERTEX_POINT ( 'NONE', #3928 ) ;
#5844 = EDGE_CURVE ( 'NONE', #4881, #2855, #5815, .T. ) ;
#5846 = CIRCLE ( 'NONE', #2303, 0.09904388296398869418 ) ;
#5847 = ORIENTED_EDGE ( 'NONE', *, *, #5901, .T. ) ;
#5848 = AXIS2_PLACEMENT_3D ( 'NONE', #6478, #811, #2000 ) ;
#5849 = EDGE_CURVE ( 'NONE', #2215, #4005, #7805, .T. ) ;
#5850 = ORIENTED_EDGE ( 'NONE', *, *, #4192, .F. ) ;
#5851 = ORIENTED_EDGE ( 'NONE', *, *, #6204, .T. ) ;
#5852 = DIRECTION ( 'NONE',  ( 0.7879377495398139919, 0.6157549048526803626, 0.000000000000000000 ) ) ;
#5853 = EDGE_LOOP ( 'NONE', ( #1296, #5626, #4157, #6160, #4242, #4889, #209, #1244, #5138, #2032 ) ) ;
#5855 = CARTESIAN_POINT ( 'NONE',  ( 1.733157827470028112, 1.373632878362779808, 0.1887011865797219856 ) ) ;
#5854 = VECTOR ( 'NONE', #2641, 39.37007874015748143 ) ;
#5856 = DIRECTION ( 'NONE',  ( 0.9987955914953421388, 0.04906492035527518225, -0.000000000000000000 ) ) ;
#5857 = VECTOR ( 'NONE', #1246, 39.37007874015748143 ) ;
#5858 = CARTESIAN_POINT ( 'NONE',  ( 0.000000000000000000, 1.425000000000000044, 0.000000000000000000 ) ) ;
#5859 = EDGE_LOOP ( 'NONE', ( #3623, #6378 ) ) ;
#5860 = DIRECTION ( 'NONE',  ( 0.000000000000000000, 0.000000000000000000, -1.000000000000000000 ) ) ;
#5861 = VECTOR ( 'NONE', #758, 39.37007874015748143 ) ;
#5862 = AXIS2_PLACEMENT_3D ( 'NONE', #4879, #1761, #2337 ) ;
#5863 = CARTESIAN_POINT ( 'NONE',  ( 1.378799321363650021, 1.727438546637902084, 0.2203823860013673641 ) ) ;
#5864 = CARTESIAN_POINT ( 'NONE',  ( -4.882388066182508091, 5.670153330992292240, 0.2179999999999999993 ) ) ;
#5865 = PERSON_AND_ORGANIZATION ( #4735, #6190 ) ;
#5866 = ORIENTED_EDGE ( 'NONE', *, *, #7091, .F. ) ;
#5867 = PLANE ( 'NONE',  #7301 ) ;
#5868 = CARTESIAN_POINT ( 'NONE',  ( -0.1249999999999999445, 0.03125000000000000000, 0.06250000000000000000 ) ) ;
#5869 = ORIENTED_EDGE ( 'NONE', *, *, #1432, .F. ) ;
#5870 = LINE ( 'NONE', #4590, #7501 ) ;
#5871 = DIRECTION ( 'NONE',  ( -0.000000000000000000, -1.000000000000000000, -0.000000000000000000 ) ) ;
#5872 = CARTESIAN_POINT ( 'NONE',  ( 1.556400554713971651, 1.293514327272109687, 0.2500000000000000000 ) ) ;
#5873 = CALENDAR_DATE ( 2026, 9, 10 ) ;
#5874 = ORIENTED_EDGE ( 'NONE', *, *, #5692, .T. ) ;
#5875 = DIRECTION ( 'NONE',  ( 0.000000000000000000, 0.000000000000000000, 1.000000000000000000 ) ) ;
#5876 = LINE ( 'NONE', #338, #4101 ) ;
#5877 = ORIENTED_EDGE ( 'NONE', *, *, #6589, .T. ) ;
#5878 = VERTEX_POINT ( 'NONE', #4505 ) ;
#5879 =( NAMED_UNIT ( * ) PLANE_ANGLE_UNIT ( ) SI_UNIT ( $, .RADIAN. ) );
#5880 = CARTESIAN_POINT ( 'NONE',  ( -0.03125000000000000000, 0.000000000000000000, -0.1162848326531996102 ) ) ;
#5881 = CARTESIAN_POINT ( 'NONE',  ( 1.475891671935536609, 0.7226544316391472211, -0.1849999999999999978 ) ) ;
#5882 = PERSON_AND_ORGANIZATION ( #524, #4145 ) ;
#5883 = CYLINDRICAL_SURFACE ( 'NONE', #2200, 0.1100000000000000006 ) ;
#5884 = DIRECTION ( 'NONE',  ( 0.000000000000000000, 1.000000000000000000, 0.000000000000000000 ) ) ;
#5885 = ORIENTED_EDGE ( 'NONE', *, *, #6921, .T. ) ;
#5886 = ORIENTED_EDGE ( 'NONE', *, *, #5550, .F. ) ;
#5887 = ADVANCED_FACE ( 'NONE', ( #5703 ), #7006, .F. ) ;
#5888 = EDGE_LOOP ( 'NONE', ( #7602, #5644, #589, #5113 ) ) ;
#5889 = ORIENTED_EDGE ( 'NONE', *, *, #1724, .F. ) ;
#5890 = ORIENTED_EDGE ( 'NONE', *, *, #1029, .T. ) ;
#5891 = DIRECTION ( 'NONE',  ( -1.000000000000000000, -1.224646799147353207E-16, 0.000000000000000000 ) ) ;
#5892 = ORIENTED_EDGE ( 'NONE', *, *, #7231, .T. ) ;
#5893 = CARTESIAN_POINT ( 'NONE',  ( 1.723083782080680360, 1.395997476760427958, 0.1965221205739619004 ) ) ;
#5894 = DIRECTION ( 'NONE',  ( 0.000000000000000000, 0.000000000000000000, -1.000000000000000000 ) ) ;
#5895 = EDGE_CURVE ( 'NONE', #6342, #7740, #6629, .T. ) ;
#5896 = EDGE_CURVE ( 'NONE', #1428, #846, #1382, .T. ) ;
#5897 = DIRECTION ( 'NONE',  ( -0.6568496200222107007, -0.7540216022612862279, 0.000000000000000000 ) ) ;
#5898 = EDGE_LOOP ( 'NONE', ( #4995, #1789, #6006, #3607 ) ) ;
#5899 = LINE ( 'NONE', #273, #6855 ) ;
#5900 = EDGE_CURVE ( 'NONE', #7153, #1621, #208, .T. ) ;
#5901 = EDGE_CURVE ( 'NONE', #3971, #2487, #5080, .T. ) ;
#5902 = VERTEX_POINT ( 'NONE', #697 ) ;
#5903 = CARTESIAN_POINT ( 'NONE',  ( 1.782722070967079242, 1.410194317043852896, 0.1437129662472861058 ) ) ;
#5904 = CC_DESIGN_PERSON_AND_ORGANIZATION_ASSIGNMENT ( #4370, #3639, ( #7233 ) ) ;
#5905 = DIRECTION ( 'NONE',  ( -1.000000000000000000, 0.000000000000000000, 0.000000000000000000 ) ) ;
#5906 = SHAPE_DEFINITION_REPRESENTATION ( #5264, #4195 ) ;
#5907 = EDGE_CURVE ( 'NONE', #4005, #3933, #4141, .T. ) ;
#5908 = DIRECTION ( 'NONE',  ( 0.000000000000000000, 0.000000000000000000, 1.000000000000000000 ) ) ;
#5909 = DIRECTION ( 'NONE',  ( 1.000000000000000000, 0.000000000000000000, 0.000000000000000000 ) ) ;
#5910 = B_SPLINE_CURVE_WITH_KNOTS ( 'NONE', 3,
 ( #253, #3416, #6651, #3379, #3495, #4107, #5918, #3450, #337, #6570, #4644, #6608 ),
 .UNSPECIFIED., .F., .F.,
 ( 4, 2, 2, 2, 2, 4 ),
 ( 0.000000000000000000, 0.0002733787321186933171, 0.0005467574642373866341, 0.001093514928474772835, 0.001640272392712158927, 0.002187029856949545235 ),
 .UNSPECIFIED. ) ;
#5911 = ORIENTED_EDGE ( 'NONE', *, *, #277, .T. ) ;
#5912 = DIRECTION ( 'NONE',  ( -0.000000000000000000, 1.000000000000000000, -0.000000000000000000 ) ) ;
#5913 = B_SPLINE_CURVE_WITH_KNOTS ( 'NONE', 3,
 ( #3631, #3011, #6212, #7437, #6169, #3747, #1197, #2502 ),
 .UNSPECIFIED., .F., .F.,
 ( 4, 2, 2, 4 ),
 ( 0.000000000000000000, 0.0003176055034687256867, 0.0006352110069374513734, 0.001270422013874900795 ),
 .UNSPECIFIED. ) ;
#5914 = CYLINDRICAL_SURFACE ( 'NONE', #2813, 0.1799999999999999933 ) ;
#5915 = LINE ( 'NONE', #289, #2450 ) ;
#5916 = DATE_AND_TIME ( #7747, #805 ) ;
#5917 = ORIENTED_EDGE ( 'NONE', *, *, #8024, .T. ) ;
#5918 = CARTESIAN_POINT ( 'NONE',  ( 0.3374272540027891121, -0.3568315896303838608, 0.2412390547417079811 ) ) ;
#5919 = PRODUCT_DEFINITION_SHAPE ( 'NONE', 'NONE',  #8100 ) ;
#5920 = DIRECTION ( 'NONE',  ( 0.000000000000000000, 0.000000000000000000, -1.000000000000000000 ) ) ;
#5921 = VERTEX_POINT ( 'NONE', #5741 ) ;
#5922 =( NAMED_UNIT ( * ) PLANE_ANGLE_UNIT ( ) SI_UNIT ( $, .RADIAN. ) );
#5923 = VERTEX_POINT ( 'NONE', #6315 ) ;
#5924 = DIRECTION ( 'NONE',  ( -1.000000000000000000, 6.975840231036812635E-15, 0.000000000000000000 ) ) ;
#5925 = PRODUCT_DEFINITION_FORMATION_WITH_SPECIFIED_SOURCE ( 'ANY', '', #7217, .NOT_KNOWN. ) ;
#5926 = CYLINDRICAL_SURFACE ( 'NONE', #7526, 0.03200000000000001454 ) ;
#5927 = VERTEX_POINT ( 'NONE', #7705 ) ;
#5928 = VECTOR ( 'NONE', #5399, 39.37007874015748143 ) ;
#5929 = EDGE_LOOP ( 'NONE', ( #5932, #6408 ) ) ;
#5930 = APPROVAL_PERSON_ORGANIZATION ( #3676, #2381, #6176 ) ;
#5931 = CARTESIAN_POINT ( 'NONE',  ( -1.222146065255383940, -0.1443597716867830172, 0.3125000000000000000 ) ) ;
#5932 = ORIENTED_EDGE ( 'NONE', *, *, #5448, .T. ) ;
#5933 = VECTOR ( 'NONE', #1769, 39.37007874015748143 ) ;
#5934 = CARTESIAN_POINT ( 'NONE',  ( 3.221700243049673507, 0.8684880333666047392, 0.1850000000000003586 ) ) ;
#5935 = CARTESIAN_POINT ( 'NONE',  ( -0.1210307295689817680, 0.6250000000000000000, -0.03125000000000000000 ) ) ;
#5936 = FACE_BOUND ( 'NONE', #7240, .T. ) ;
#5937 = DIRECTION ( 'NONE',  ( -0.2791259188691606608, -0.9602545086670756236, -0.000000000000000000 ) ) ;
#5938 = AXIS2_PLACEMENT_3D ( 'NONE', #2689, #3309, #7077 ) ;
#5939 = CARTESIAN_POINT ( 'NONE',  ( 2.204364238465235822E-17, 0.000000000000000000, 0.1799999999999999933 ) ) ;
#5940 = DIRECTION ( 'NONE',  ( -1.000000000000000000, -1.762482576557733776E-15, 0.000000000000000000 ) ) ;
#5941 = EDGE_CURVE ( 'NONE', #6082, #2455, #2649, .T. ) ;
#5942 = TOROIDAL_SURFACE ( 'NONE', #2397, 0.2112499999999999933, 0.03125000000000000000 ) ;
#5943 = LINE ( 'NONE', #5987, #1781 ) ;
#5944 = ORIENTED_EDGE ( 'NONE', *, *, #3338, .T. ) ;
#5945 = EDGE_CURVE ( 'NONE', #3903, #7979, #2536, .T. ) ;
#5946 = DIRECTION ( 'NONE',  ( 0.3151807705563068884, 0.2463063934922189724, -0.9165119979555036434 ) ) ;
#5947 = CC_DESIGN_PERSON_AND_ORGANIZATION_ASSIGNMENT ( #3218, #5723, ( #4611 ) ) ;
#5948 = ADVANCED_FACE ( 'NONE', ( #4550 ), #5041, .F. ) ;
#5949 = AXIS2_PLACEMENT_3D ( 'NONE', #1500, #5194, #5852 ) ;
#5950 = ADVANCED_FACE ( 'NONE', ( #7081 ), #874, .T. ) ;
#5951 = LINE ( 'NONE', #1473, #3464 ) ;
#5952 = CARTESIAN_POINT ( 'NONE',  ( 1.518108166580419915, 1.876045830693510164, 0.0007282234754631174015 ) ) ;
#5953 = APPROVAL_STATUS ( 'not_yet_approved' ) ;
#5954 = VERTEX_POINT ( 'NONE', #3271 ) ;
#5955 = DIRECTION ( 'NONE',  ( 0.7540216022612858948, -0.6568496200222110337, 0.000000000000000000 ) ) ;
#5956 = CARTESIAN_POINT ( 'NONE',  ( 1.328121161265039207, 1.072473730611112064, -0.1194156274346386548 ) ) ;
#5957 = AXIS2_PLACEMENT_3D ( 'NONE', #1031, #2904, #6766 ) ;
#5958 = DIRECTION ( 'NONE',  ( 0.000000000000000000, 1.000000000000000000, 0.000000000000000000 ) ) ;
#5959 = EDGE_LOOP ( 'NONE', ( #4211, #6056, #3566, #4663 ) ) ;
#5960 = AXIS2_PLACEMENT_3D ( 'NONE', #2126, #2651, #1620 ) ;
#5961 = ORIENTED_EDGE ( 'NONE', *, *, #1284, .T. ) ;
#5962 = VECTOR ( 'NONE', #5079, 39.37007874015748143 ) ;
#5963 = ORIENTED_EDGE ( 'NONE', *, *, #1273, .T. ) ;
#5964 = CARTESIAN_POINT ( 'NONE',  ( 0.9887166869077879117, 0.8277708867933823988, 0.03199999999999999373 ) ) ;
#5965 = DIRECTION ( 'NONE',  ( -0.7879377495398141029, -0.6157549048526801405, 0.000000000000000000 ) ) ;
#5966 = PERSON_AND_ORGANIZATION ( #936, #580 ) ;
#5967 = DIRECTION ( 'NONE',  ( -0.000000000000000000, -1.000000000000000000, -0.000000000000000000 ) ) ;
#5968 = ORIENTED_EDGE ( 'NONE', *, *, #428, .T. ) ;
#5969 = AXIS2_PLACEMENT_3D ( 'NONE', #4046, #6548, #420 ) ;
#5970 = ORIENTED_EDGE ( 'NONE', *, *, #6257, .T. ) ;
#5971 = FACE_OUTER_BOUND ( 'NONE', #1663, .T. ) ;
#5972 = VECTOR ( 'NONE', #4683, 39.37007874015747433 ) ;
#5973 = UNCERTAINTY_MEASURE_WITH_UNIT (LENGTH_MEASURE( 1.000000000000000082E-05 ), #127, 'distance_accuracy_value', 'NONE');
#5974 = CARTESIAN_POINT ( 'NONE',  ( 0.000000000000000000, 0.000000000000000000, -0.6849999999999999423 ) ) ;
#5975 = CARTESIAN_POINT ( 'NONE',  ( -0.1054677083281892608, 0.000000000000000000, -0.03125000000000000000 ) ) ;
#5976 = VERTEX_POINT ( 'NONE', #6475 ) ;
#5977 = CIRCLE ( 'NONE', #86, 0.1250000000000001388 ) ;
#5978 = CARTESIAN_POINT ( 'NONE',  ( 3.672798492683009286, -8.252032378159654513, 5.393636709996481038 ) ) ;
#5979 = CARTESIAN_POINT ( 'NONE',  ( 0.1250000000000000000, 0.000000000000000000, 0.000000000000000000 ) ) ;
#5980 = CIRCLE ( 'NONE', #736, 0.1249999999999999029 ) ;
#5981 = ORIENTED_EDGE ( 'NONE', *, *, #3991, .T. ) ;
#5982 = ORIENTED_EDGE ( 'NONE', *, *, #4846, .T. ) ;
#5983 = AXIS2_PLACEMENT_3D ( 'NONE', #5779, #2748, #3247 ) ;
#5984 = PRODUCT_DEFINITION_SHAPE ( 'NONE', 'NONE',  #3498 ) ;
#5985 = DIRECTION ( 'NONE',  ( 0.000000000000000000, 0.000000000000000000, -1.000000000000000000 ) ) ;
#5986 = CARTESIAN_POINT ( 'NONE',  ( -0.1249999999999999445, -0.03125000000000000000, 0.06250000000000000000 ) ) ;
#5987 = CARTESIAN_POINT ( 'NONE',  ( -1.763630694164994850, 1.150051601412733771, 0.1649762307749162715 ) ) ;
#5988 = ORIENTED_EDGE ( 'NONE', *, *, #6298, .F. ) ;
#5989 = CIRCLE ( 'NONE', #4424, 0.01652128394798136474 ) ;
#5990 = DIRECTION ( 'NONE',  ( -0.000000000000000000, -1.000000000000000000, -0.000000000000000000 ) ) ;
#5991 = EDGE_CURVE ( 'NONE', #7663, #3956, #344, .T. ) ;
#5992 = EDGE_CURVE ( 'NONE', #5067, #7187, #4824, .T. ) ;
#5993 = AXIS2_PLACEMENT_3D ( 'NONE', #2719, #7682, #2757 ) ;
#5994 = DIRECTION ( 'NONE',  ( 0.000000000000000000, -0.000000000000000000, -1.000000000000000000 ) ) ;
#5995 =( REPRESENTATION_RELATIONSHIP ('NONE','NONE', #3360, #1942 ) REPRESENTATION_RELATIONSHIP_WITH_TRANSFORMATION ( #349 )SHAPE_REPRESENTATION_RELATIONSHIP( ) );
#5996 = VECTOR ( 'NONE', #4147, 39.37007874015748143 ) ;
#5997 = CARTESIAN_POINT ( 'NONE',  ( 1.492768560906099662, 1.856243522084602304, -0.0006067816429719980484 ) ) ;
#5998 = PERSON_AND_ORGANIZATION ( #4735, #6190 ) ;
#5999 = ORIENTED_EDGE ( 'NONE', *, *, #4180, .F. ) ;
#6000 = DIRECTION ( 'NONE',  ( -0.6157549048526804736, 0.7879377495398138809, 0.000000000000000000 ) ) ;
#6001 = PRODUCT_DEFINITION ( 'UNKNOWN', '', #4083, #2765 ) ;
#6002 = CARTESIAN_POINT ( 'NONE',  ( 1.566033889679777413, 1.280741487518077371, 0.2500000000000000555 ) ) ;
#6003 = EDGE_CURVE ( 'NONE', #6740, #1607, #6246, .T. ) ;
#6004 = ORIENTED_EDGE ( 'NONE', *, *, #5896, .T. ) ;
#6005 = EDGE_CURVE ( 'NONE', #1614, #4959, #5059, .T. ) ;
#6006 = ORIENTED_EDGE ( 'NONE', *, *, #5696, .F. ) ;
#6007 = ORIENTED_EDGE ( 'NONE', *, *, #5539, .T. ) ;
#6008 = ORIENTED_EDGE ( 'NONE', *, *, #2989, .F. ) ;
#6009 = DIRECTION ( 'NONE',  ( 0.7879377495398141029, 0.6157549048526802515, 0.000000000000000000 ) ) ;
#6010 = CARTESIAN_POINT ( 'NONE',  ( 1.452776126471488682, 1.185506347943134475, 0.2257575757576623099 ) ) ;
#6011 = COORDINATED_UNIVERSAL_TIME_OFFSET ( 0, 0, .AHEAD. ) ;
#6012 = CARTESIAN_POINT ( 'NONE',  ( -1.803041671366328202, 1.104810305277057259, -0.3269762307749163877 ) ) ;
#6013 = ORIENTED_EDGE ( 'NONE', *, *, #4182, .F. ) ;
#6014 = ORIENTED_EDGE ( 'NONE', *, *, #6936, .F. ) ;
#6015 = CARTESIAN_POINT ( 'NONE',  ( 0.2796912674003787513, -4.528516545235624413, 0.2500000000000000000 ) ) ;
#6016 = PLANE ( 'NONE',  #7383 ) ;
#6017 = CARTESIAN_POINT ( 'NONE',  ( 1.353765837681602191, 0.002299485657152759710, -0.1250000000000000278 ) ) ;
#6018 = DIRECTION ( 'NONE',  ( 1.000000000000000000, 0.000000000000000000, 0.000000000000000000 ) ) ;
#6019 = ORIENTED_EDGE ( 'NONE', *, *, #3381, .T. ) ;
#6020 = CARTESIAN_POINT ( 'NONE',  ( 6.067386035484801710, 0.2407470087491039856, 0.1250000000000000000 ) ) ;
#6021 = DIRECTION ( 'NONE',  ( -0.000000000000000000, -0.000000000000000000, 1.000000000000000000 ) ) ;
#6022 = FACE_OUTER_BOUND ( 'NONE', #6648, .T. ) ;
#6023 = CARTESIAN_POINT ( 'NONE',  ( 6.067385397437120353, 0.2407432673787524013, -0.1849999999999999978 ) ) ;
#6024 = FACE_OUTER_BOUND ( 'NONE', #1173, .T. ) ;
#6025 = ORIENTED_EDGE ( 'NONE', *, *, #6442, .F. ) ;
#6026 = DIRECTION ( 'NONE',  ( 0.000000000000000000, 0.000000000000000000, 1.000000000000000000 ) ) ;
#6027 = FACE_OUTER_BOUND ( 'NONE', #5853, .T. ) ;
#6028 = CARTESIAN_POINT ( 'NONE',  ( 1.142655413120957197, 0.6307864494084283180, 0.2179999999999999993 ) ) ;
#6029 = APPLICATION_PROTOCOL_DEFINITION ( 'international standard', 'config_control_design', 1994, #1369 ) ;
#6030 = ORIENTED_EDGE ( 'NONE', *, *, #4589, .F. ) ;
#6031 = DIRECTION ( 'NONE',  ( 0.000000000000000000, -0.000000000000000000, -1.000000000000000000 ) ) ;
#6032 = CARTESIAN_POINT ( 'NONE',  ( 0.000000000000000000, 0.000000000000000000, -0.6229999999999998872 ) ) ;
#6033 = EDGE_CURVE ( 'NONE', #5382, #1614, #7733, .T. ) ;
#6034 = CARTESIAN_POINT ( 'NONE',  ( 0.000000000000000000, 1.081250000000000044, 0.000000000000000000 ) ) ;
#6035 = EDGE_LOOP ( 'NONE', ( #4331, #6799, #4187, #7134 ) ) ;
#6036 = EDGE_LOOP ( 'NONE', ( #1608, #7197, #1158, #3753 ) ) ;
#6037 = VERTEX_POINT ( 'NONE', #913 ) ;
#6038 = ORIENTED_EDGE ( 'NONE', *, *, #4734, .F. ) ;
#6039 = DIRECTION ( 'NONE',  ( 0.000000000000000000, -1.000000000000000000, 0.000000000000000000 ) ) ;
#6040 = CARTESIAN_POINT ( 'NONE',  ( 1.380988422954957606, 1.174934410395800821, 0.2500000000000000000 ) ) ;
#6041 = SECURITY_CLASSIFICATION_LEVEL ( 'unclassified' ) ;
#6042 = CARTESIAN_POINT ( 'NONE',  ( 0.9690125299525020885, 0.8529848947786566882, 0.000000000000000000 ) ) ;
#6043 = EDGE_CURVE ( 'NONE', #3239, #3428, #2692, .T. ) ;
#6044 = CC_DESIGN_APPROVAL ( #2585, ( #6696 ) ) ;
#6045 = CC_DESIGN_APPROVAL ( #3935, ( #7483 ) ) ;
#6046 = EDGE_CURVE ( 'NONE', #2261, #1684, #2245, .T. ) ;
#6047 = CC_DESIGN_PERSON_AND_ORGANIZATION_ASSIGNMENT ( #7476, #2977, ( #4024 ) ) ;
#6048 = EDGE_CURVE ( 'NONE', #7906, #810, #7283, .T. ) ;
#6049 = APPROVAL_PERSON_ORGANIZATION ( #5497, #6496, #4923 ) ;
#6050 = CARTESIAN_POINT ( 'NONE',  ( 0.1028096983035132889, -0.4582465879184300372, 0.03199999999999999373 ) ) ;
#6051 = PLANE ( 'NONE',  #2401 ) ;
#6052 = APPROVAL_STATUS ( 'not_yet_approved' ) ;
#6053 = LINE ( 'NONE', #1745, #223 ) ;
#6054 = DIRECTION ( 'NONE',  ( -0.000000000000000000, -0.000000000000000000, -1.000000000000000000 ) ) ;
#6055 = AXIS2_PLACEMENT_3D ( 'NONE', #7479, #2619, #4564 ) ;
#6056 = ORIENTED_EDGE ( 'NONE', *, *, #5844, .F. ) ;
#6057 = DIRECTION ( 'NONE',  ( 0.6568496200222107007, 0.7540216022612863389, 0.000000000000000000 ) ) ;
#6058 =( GEOMETRIC_REPRESENTATION_CONTEXT ( 3 ) GLOBAL_UNCERTAINTY_ASSIGNED_CONTEXT ( ( #6862 ) ) GLOBAL_UNIT_ASSIGNED_CONTEXT ( ( #7989, #4816, #6689 ) ) REPRESENTATION_CONTEXT ( 'NONE', 'WORKASPACE' ) );
#6059 = CARTESIAN_POINT ( 'NONE',  ( 0.03125000000000000000, -0.03125000000000000000, 0.1162848326531996102 ) ) ;
#6060 = CIRCLE ( 'NONE', #2384, 0.06250000000000000000 ) ;
#6061 = LOCAL_TIME ( 14, 45, 32.00000000000000000, #1475 ) ;
#6062 = DIRECTION ( 'NONE',  ( 0.000000000000000000, 0.000000000000000000, 1.000000000000000000 ) ) ;
#6063 = DIRECTION ( 'NONE',  ( 0.000000000000000000, -0.000000000000000000, -1.000000000000000000 ) ) ;
#6064 = CARTESIAN_POINT ( 'NONE',  ( 0.8923633780935225079, 0.7607014108325281798, 0.000000000000000000 ) ) ;
#6065 = EDGE_LOOP ( 'NONE', ( #1615, #3096, #1662, #535, #7222 ) ) ;
#6066 = CIRCLE ( 'NONE', #5938, 0.03125000000000000694 ) ;
#6067 = EDGE_LOOP ( 'NONE', ( #613, #2602, #4109, #346 ) ) ;
#6068 = CARTESIAN_POINT ( 'NONE',  ( 0.000000000000000000, 1.393749999999999822, 0.1487499999999999933 ) ) ;
#6069 = VECTOR ( 'NONE', #2396, 39.37007874015748854 ) ;
#6070 = FACE_OUTER_BOUND ( 'NONE', #4039, .T. ) ;
#6071 = DIRECTION ( 'NONE',  ( -0.6568496200222107007, -0.7540216022612862279, 0.000000000000000000 ) ) ;
#6072 = PERSON_AND_ORGANIZATION ( #4735, #6190 ) ;
#6073 = ORIENTED_EDGE ( 'NONE', *, *, #6936, .T. ) ;
#6074 = CARTESIAN_POINT ( 'NONE',  ( -1.411841654243101596, 0.8435981834898315102, -0.1250000000000000000 ) ) ;
#6075 = DIRECTION ( 'NONE',  ( -0.000000000000000000, -0.000000000000000000, 1.000000000000000000 ) ) ;
#6076 = CARTESIAN_POINT ( 'NONE',  ( -0.06999999999999996503, -0.03125000000000000000, 0.8125000000000000000 ) ) ;
#6077 = VECTOR ( 'NONE', #3429, 39.37007874015748143 ) ;
#6078 = AXIS2_PLACEMENT_3D ( 'NONE', #7799, #6009, #7833 ) ;
#6079 = ORIENTED_EDGE ( 'NONE', *, *, #4887, .T. ) ;
#6080 = CC_DESIGN_APPROVAL ( #5699, ( #51 ) ) ;
#6081 =( LENGTH_UNIT ( ) NAMED_UNIT ( * ) SI_UNIT ( $, .METRE. ) );
#6082 = VERTEX_POINT ( 'NONE', #5986 ) ;
#6083 = CARTESIAN_POINT ( 'NONE',  ( 6.190240298342082781, 0.4584752965318060758, 0.000000000000000000 ) ) ;
#6084 = CIRCLE ( 'NONE', #5684, 0.09507037842118626347 ) ;
#6085 = CARTESIAN_POINT ( 'NONE',  ( 0.09078267040543826216, -0.4599203499726461364, 0.2266307369244480729 ) ) ;
#6086 = PERSON_AND_ORGANIZATION_ROLE ( 'classification_officer' ) ;
#6087 = CARTESIAN_POINT ( 'NONE',  ( 2.387087291339119677, -6.013863021948615106, -0.1250000000000000000 ) ) ;
#6088 = ORIENTED_EDGE ( 'NONE', *, *, #2679, .T. ) ;
#6089 = CLOSED_SHELL ( 'NONE', ( #4447, #6828, #816, #586, #6587, #1629, #4840, #2426, #3144, #1819, #3432, #7943, #7392, #3837, #7101 ) ) ;
#6090 = VECTOR ( 'NONE', #2747, 39.37007874015748143 ) ;
#6091 = EDGE_CURVE ( 'NONE', #4570, #3425, #5846, .T. ) ;
#6092 = ORIENTED_EDGE ( 'NONE', *, *, #994, .T. ) ;
#6093 = EDGE_CURVE ( 'NONE', #7191, #4234, #3751, .T. ) ;
#6094 = EDGE_CURVE ( 'NONE', #6811, #7764, #2213, .T. ) ;
#6095 = DIRECTION ( 'NONE',  ( -0.000000000000000000, -0.000000000000000000, -1.000000000000000000 ) ) ;
#6096 = CARTESIAN_POINT ( 'NONE',  ( -6.057578121783967262, -1.099253028489540318, 0.3125000000000000000 ) ) ;
#6097 = CARTESIAN_POINT ( 'NONE',  ( -0.3566525292043903339, -0.3408511508279103985, -0.1250000000000000000 ) ) ;
#6098 = APPROVAL_ROLE ( '' ) ;
#6099 = CARTESIAN_POINT ( 'NONE',  ( -0.1250000000000000000, 0.6250000000000000000, -0.03125000000000000000 ) ) ;
#6100 = DIRECTION ( 'NONE',  ( -1.000000000000000000, 0.000000000000000000, 0.000000000000000000 ) ) ;
#6101 = VECTOR ( 'NONE', #2231, 39.37007874015748143 ) ;
#6102 = AXIS2_PLACEMENT_3D ( 'NONE', #3112, #2444, #7530 ) ;
#6103 = ORIENTED_EDGE ( 'NONE', *, *, #4444, .F. ) ;
#6104 = PRODUCT_RELATED_PRODUCT_CATEGORY ( 'detail', '', ( #2761 ) ) ;
#6105 = FACE_OUTER_BOUND ( 'NONE', #1739, .T. ) ;
#6106 = ADVANCED_FACE ( 'NONE', ( #7176 ), #7779, .T. ) ;
#6107 = FACE_OUTER_BOUND ( 'NONE', #3161, .T. ) ;
#6108 = CIRCLE ( 'NONE', #7287, 0.03200000000000003536 ) ;
#6109 = CARTESIAN_POINT ( 'NONE',  ( 0.3566525292043903339, -0.3408511508279103985, 0.2179999999999999993 ) ) ;
#6110 = CARTESIAN_POINT ( 'NONE',  ( 1.353740795342264880, 0.002292344206096672693, 0.1250000000000592026 ) ) ;
#6111 = CARTESIAN_POINT ( 'NONE',  ( 0.6597999294535048520, -0.04777128394798136474, 0.000000000000000000 ) ) ;
#6112 = CIRCLE ( 'NONE', #4930, 0.06199999999999999956 ) ;
#6113 = ORIENTED_EDGE ( 'NONE', *, *, #4377, .F. ) ;
#6114 = ORIENTED_EDGE ( 'NONE', *, *, #7630, .F. ) ;
#6115 = CARTESIAN_POINT ( 'NONE',  ( 1.846835003037430534, 1.498370261438588313, 0.03199999999999999373 ) ) ;
#6116 = AXIS2_PLACEMENT_3D ( 'NONE', #7248, #322, #4097 ) ;
#6117 = AXIS2_PLACEMENT_3D ( 'NONE', #1513, #6530, #5908 ) ;
#6118 = CARTESIAN_POINT ( 'NONE',  ( -0.9142296270274480330, 0.5739542246721696106, 0.1250000000000000000 ) ) ;
#6119 = DIRECTION ( 'NONE',  ( 0.000000000000000000, 0.000000000000000000, 1.000000000000000000 ) ) ;
#6120 = DATE_TIME_ROLE ( 'creation_date' ) ;
#6121 = EDGE_LOOP ( 'NONE', ( #4210, #4405, #6851, #2714 ) ) ;
#6122 = FACE_OUTER_BOUND ( 'NONE', #7684, .T. ) ;
#6123 = AXIS2_PLACEMENT_3D ( 'NONE', #7562, #7628, #755 ) ;
#6124 = CARTESIAN_POINT ( 'NONE',  ( 0.000000000000000000, 0.000000000000000000, 0.000000000000000000 ) ) ;
#6125 = DIRECTION ( 'NONE',  ( -0.000000000000000000, 0.000000000000000000, -1.000000000000000000 ) ) ;
#6126 = VECTOR ( 'NONE', #5842, 39.37007874015748854 ) ;
#6127 = ORIENTED_EDGE ( 'NONE', *, *, #7281, .T. ) ;
#6128 = CARTESIAN_POINT ( 'NONE',  ( 0.2386870781737283065, -0.03125000000000000000, 0.07449999999999999678 ) ) ;
#6129 = ORIENTED_EDGE ( 'NONE', *, *, #3990, .T. ) ;
#6130 = CARTESIAN_POINT ( 'NONE',  ( 0.9887166869077879117, 0.8277708867933823988, 0.2500000000000000000 ) ) ;
#6131 = CALENDAR_DATE ( 2026, 9, 10 ) ;
#6132 = CARTESIAN_POINT ( 'NONE',  ( 0.000000000000000000, 0.03125000000000000000, 0.6646281645421511231 ) ) ;
#6133 = ORIENTED_EDGE ( 'NONE', *, *, #2926, .T. ) ;
#6134 = ORIENTED_EDGE ( 'NONE', *, *, #7085, .F. ) ;
#6135 = CARTESIAN_POINT ( 'NONE',  ( 1.652539028737726179, 1.219618926967090289, -0.1039999999999998703 ) ) ;
#6136 = CARTESIAN_POINT ( 'NONE',  ( 0.02822771919327313195, 0.03615965030275954117, 0.000000000000000000 ) ) ;
#6137 = DIRECTION ( 'NONE',  ( 0.000000000000000000, -0.000000000000000000, -1.000000000000000000 ) ) ;
#6138 = COORDINATED_UNIVERSAL_TIME_OFFSET ( 0, 0, .AHEAD. ) ;
#6139 = DIRECTION ( 'NONE',  ( -1.000000000000000000, 0.000000000000000000, 0.000000000000000000 ) ) ;
#6140 = DIRECTION ( 'NONE',  ( -1.000000000000000000, -0.000000000000000000, -0.000000000000000000 ) ) ;
#6141 = ORIENTED_EDGE ( 'NONE', *, *, #5837, .F. ) ;
#6142 = CARTESIAN_POINT ( 'NONE',  ( 1.608451107215755904, 1.301813166848322822, 0.2376577216243210278 ) ) ;
#6143 = EDGE_CURVE ( 'NONE', #4660, #5314, #478, .T. ) ;
#6144 = PLANE ( 'NONE',  #443 ) ;
#6145 = ORIENTED_EDGE ( 'NONE', *, *, #7200, .F. ) ;
#6146 = CARTESIAN_POINT ( 'NONE',  ( 1.515917799388286635, 1.833721764662388232, -0.1039999999999998703 ) ) ;
#6147 = ADVANCED_FACE ( 'NONE', ( #2173 ), #7160, .T. ) ;
#6148 = CARTESIAN_POINT ( 'NONE',  ( 1.283278058574945257, 1.059461569165262462, -0.07928749764790786470 ) ) ;
#6149 = DIRECTION ( 'NONE',  ( 0.7879377495398141029, 0.6157549048526802515, 0.000000000000000000 ) ) ;
#6150 = EDGE_CURVE ( 'NONE', #3851, #518, #1005, .T. ) ;
#6151 = ORIENTED_EDGE ( 'NONE', *, *, #1235, .F. ) ;
#6152 = EDGE_CURVE ( 'NONE', #4276, #4081, #1524, .T. ) ;
#6153 = CARTESIAN_POINT ( 'NONE',  ( 1.544745509581308296, 0.8307882251580827049, -0.08212881570848259982 ) ) ;
#6154 = DIMENSIONAL_EXPONENTS ( 1.000000000000000000, 0.000000000000000000, 0.000000000000000000, 0.000000000000000000, 0.000000000000000000, 0.000000000000000000, 0.000000000000000000 ) ;
#6155 = CC_DESIGN_PERSON_AND_ORGANIZATION_ASSIGNMENT ( #2125, #5434, ( #5925 ) ) ;
#6156 = EDGE_CURVE ( 'NONE', #713, #3658, #5977, .T. ) ;
#6157 = PLANE ( 'NONE',  #3994 ) ;
#6158 = DIRECTION ( 'NONE',  ( 0.4964005096718474008, 0.8680936205257645533, 0.000000000000000000 ) ) ;
#6159 = SECURITY_CLASSIFICATION_LEVEL ( 'unclassified' ) ;
#6160 = ORIENTED_EDGE ( 'NONE', *, *, #5696, .T. ) ;
#6161 = FACE_BOUND ( 'NONE', #7678, .T. ) ;
#6162 = CARTESIAN_POINT ( 'NONE',  ( -1.411841654243101596, 0.8435981834898315102, 0.1250000000000000000 ) ) ;
#6163 = ORIENTED_EDGE ( 'NONE', *, *, #5217, .F. ) ;
#6164 = DIRECTION ( 'NONE',  ( 0.000000000000000000, 0.000000000000000000, 1.000000000000000000 ) ) ;
#6165 = ORIENTED_EDGE ( 'NONE', *, *, #6756, .T. ) ;
#6166 = DIRECTION ( 'NONE',  ( 0.6157549048526804736, -0.7879377495398138809, 0.000000000000000000 ) ) ;
#6167 = DIRECTION ( 'NONE',  ( -0.000000000000000000, -0.000000000000000000, -1.000000000000000000 ) ) ;
#6168 = COORDINATED_UNIVERSAL_TIME_OFFSET ( 0, 0, .AHEAD. ) ;
#6169 = CARTESIAN_POINT ( 'NONE',  ( -1.042831394347257357, -0.7466732791099464084, 0.2376747752564828120 ) ) ;
#6170 = VERTEX_POINT ( 'NONE', #4134 ) ;
#6171 = ORIENTED_EDGE ( 'NONE', *, *, #4695, .F. ) ;
#6172 = ORIENTED_EDGE ( 'NONE', *, *, #3188, .F. ) ;
#6173 = DIRECTION ( 'NONE',  ( 1.000000000000000000, 0.000000000000000000, 0.000000000000000000 ) ) ;
#6174 = CARTESIAN_POINT ( 'NONE',  ( 0.000000000000000000, 0.000000000000000000, -0.6849999999999999423 ) ) ;
#6175 = CARTESIAN_POINT ( 'NONE',  ( 0.1024500231158892299, -0.4583009483847821364, 0.03046749565051176320 ) ) ;
#6176 = APPROVAL_ROLE ( '' ) ;
#6177 = DIRECTION ( 'NONE',  ( -1.000000000000000000, 0.000000000000000000, 0.000000000000000000 ) ) ;
#6178 = CARTESIAN_POINT ( 'NONE',  ( 1.658388808675685056, 1.714694511436468005, 1.938114344956973572E-14 ) ) ;
#6179 = CARTESIAN_POINT ( 'NONE',  ( 1.591243317659689405, 1.252944055095702725, 0.2002330193986645301 ) ) ;
#6180 = CC_DESIGN_APPROVAL ( #7704, ( #172 ) ) ;
#6181 = EDGE_CURVE ( 'NONE', #6698, #898, #1136, .T. ) ;
#6182 = EDGE_LOOP ( 'NONE', ( #239, #2002, #4539, #7951, #6769, #5505 ) ) ;
#6183 = DIRECTION ( 'NONE',  ( 0.000000000000000000, 0.000000000000000000, 1.000000000000000000 ) ) ;
#6184 = DIRECTION ( 'NONE',  ( 0.000000000000000000, 0.000000000000000000, -1.000000000000000000 ) ) ;
#6185 = DIRECTION ( 'NONE',  ( 0.000000000000000000, 1.000000000000000000, 0.000000000000000000 ) ) ;
#6186 = ORIENTED_EDGE ( 'NONE', *, *, #215, .T. ) ;
#6187 = ORIENTED_EDGE ( 'NONE', *, *, #691, .F. ) ;
#6188 = LINE ( 'NONE', #1220, #3052 ) ;
#6189 = CIRCLE ( 'NONE', #7229, 0.03124999999999999306 ) ;
#6190 = ORGANIZATION ( 'UNSPECIFIED', 'UNSPECIFIED', '' ) ;
#6191 = EDGE_CURVE ( 'NONE', #2684, #7370, #397, .T. ) ;
#6192 = EDGE_CURVE ( 'NONE', #3726, #6549, #2428, .T. ) ;
#6193 = EDGE_CURVE ( 'NONE', #1300, #4722, #3774, .T. ) ;
#6194 = FACE_OUTER_BOUND ( 'NONE', #4814, .T. ) ;
#6195 = DIRECTION ( 'NONE',  ( 0.000000000000000000, 0.000000000000000000, 1.000000000000000000 ) ) ;
#6196 = DATE_AND_TIME ( #567, #3556 ) ;
#6197 = ORIENTED_EDGE ( 'NONE', *, *, #832, .F. ) ;
#6198 = EDGE_CURVE ( 'NONE', #1380, #5139, #4380, .T. ) ;
#6199 = AXIS2_PLACEMENT_3D ( 'NONE', #4038, #7186, #2300 ) ;
#6200 = FACE_OUTER_BOUND ( 'NONE', #677, .T. ) ;
#6201 = CARTESIAN_POINT ( 'NONE',  ( 6.185915932928153005, 0.4597367884986204856, 0.000000000000000000 ) ) ;
#6202 = EDGE_LOOP ( 'NONE', ( #1446, #5869, #7748, #3354 ) ) ;
#6203 = APPROVAL ( #4162, 'UNKNOWN' ) ;
#6204 = EDGE_CURVE ( 'NONE', #2424, #6313, #3649, .T. ) ;
#6205 = ADVANCED_FACE ( 'NONE', ( #1144 ), #557, .F. ) ;
#6206 = AXIS2_PLACEMENT_3D ( 'NONE', #5369, #6524, #4579 ) ;
#6207 = ORIENTED_EDGE ( 'NONE', *, *, #5794, .T. ) ;
#6208 = DIRECTION ( 'NONE',  ( -0.000000000000000000, 0.000000000000000000, 1.000000000000000000 ) ) ;
#6209 = CARTESIAN_POINT ( 'NONE',  ( 0.7938352818576230874, 1.310043527237014560, 0.03200000000000000067 ) ) ;
#6210 = DIMENSIONAL_EXPONENTS ( 1.000000000000000000, 0.000000000000000000, 0.000000000000000000, 0.000000000000000000, 0.000000000000000000, 0.000000000000000000, 0.000000000000000000 ) ;
#6211 = SECURITY_CLASSIFICATION_LEVEL ( 'unclassified' ) ;
#6212 = CARTESIAN_POINT ( 'NONE',  ( -1.041235186073524277, -0.7520349028915425116, 0.2263769898119324941 ) ) ;
#6213 = VECTOR ( 'NONE', #3087, 39.37007874015748143 ) ;
#6214 = EDGE_CURVE ( 'NONE', #5222, #1079, #7418, .T. ) ;
#6215 = AXIS2_PLACEMENT_3D ( 'NONE', #5365, #1090, #310 ) ;
#6216 = AXIS2_PLACEMENT_3D ( 'NONE', #7235, #5364, #3427 ) ;
#6217 = VERTEX_POINT ( 'NONE', #6759 ) ;
#6218 = CYLINDRICAL_SURFACE ( 'NONE', #7777, 0.3099400561648077423 ) ;
#6219 = DIRECTION ( 'NONE',  ( -1.000000000000000000, 0.000000000000000000, 0.000000000000000000 ) ) ;
#6220 = UNCERTAINTY_MEASURE_WITH_UNIT (LENGTH_MEASURE( 1.000000000000000082E-05 ), #2225, 'distance_accuracy_value', 'NONE');
#6221 = CARTESIAN_POINT ( 'NONE',  ( 0.000000000000000000, -0.03125000000000000000, 0.6811494484901324808 ) ) ;
#6222 = DATE_TIME_ROLE ( 'creation_date' ) ;
#6223 = CARTESIAN_POINT ( 'NONE',  ( 1.258616367985684104, -0.02482036785324303815, 0.1250000000000000000 ) ) ;
#6224 = CARTESIAN_POINT ( 'NONE',  ( 1.904163605026766071, 1.432560671222282922, -6.829619984160658046E-16 ) ) ;
#6225 = ORIENTED_EDGE ( 'NONE', *, *, #7394, .F. ) ;
#6226 = CARTESIAN_POINT ( 'NONE',  ( 1.725603453493498973, 1.399212170159634283, 0.2321060441915416273 ) ) ;
#6227 = LOCAL_TIME ( 14, 45, 32.00000000000000000, #4362 ) ;
#6228 = CIRCLE ( 'NONE', #7396, 0.2499400561648078278 ) ;
#6229 = ORIENTED_EDGE ( 'NONE', *, *, #3891, .T. ) ;
#6230 = LINE ( 'NONE', #519, #7653 ) ;
#6231 = CARTESIAN_POINT ( 'NONE',  ( 1.322797517748710572, 1.071418997054937261, -0.08446866672460882908 ) ) ;
#6232 = CARTESIAN_POINT ( 'NONE',  ( 1.380988422954957606, 1.174934410395800821, 0.2500000000000000000 ) ) ;
#6233 = ORIENTED_EDGE ( 'NONE', *, *, #2991, .T. ) ;
#6234 = ORIENTED_EDGE ( 'NONE', *, *, #6494, .T. ) ;
#6235 = FACE_OUTER_BOUND ( 'NONE', #840, .T. ) ;
#6236 = TOROIDAL_SURFACE ( 'NONE', #7406, 0.1523203157102362704, 0.06250000000000000000 ) ;
#6237 = ORIENTED_EDGE ( 'NONE', *, *, #6840, .F. ) ;
#6238 = DIRECTION ( 'NONE',  ( -6.975840231036812635E-15, -1.000000000000000000, 2.013666839457971600E-30 ) ) ;
#6239 = CARTESIAN_POINT ( 'NONE',  ( -6.163625881728066247, -1.710116247721755522, 0.3125000000000000000 ) ) ;
#6240 = CIRCLE ( 'NONE', #4528, 0.3045082206899650812 ) ;
#6241 = APPROVAL_DATE_TIME ( #1960, #1185 ) ;
#6242 = VERTEX_POINT ( 'NONE', #5569 ) ;
#6243 = SPHERICAL_SURFACE ( 'NONE', #7691, 0.1150000000000000050 ) ;
#6244 = CARTESIAN_POINT ( 'NONE',  ( -0.04782642554762442377, -0.07812500000000000000, 0.07449999999999999678 ) ) ;
#6245 = ORIENTED_EDGE ( 'NONE', *, *, #2374, .F. ) ;
#6246 = CIRCLE ( 'NONE', #7546, 8.696493751522730520 ) ;
#6247 = FACE_OUTER_BOUND ( 'NONE', #2203, .T. ) ;
#6248 = CIRCLE ( 'NONE', #2837, 0.2148203157102362704 ) ;
#6249 = ADVANCED_FACE ( 'NONE', ( #7454, #4987, #7936 ), #1215, .F. ) ;
#6250 = EDGE_CURVE ( 'NONE', #375, #658, #3763, .T. ) ;
#6251 = VECTOR ( 'NONE', #2331, 39.37007874015748143 ) ;
#6252 = VERTEX_POINT ( 'NONE', #4835 ) ;
#6253 = CIRCLE ( 'NONE', #8055, 0.3099400561648077423 ) ;
#6254 = CARTESIAN_POINT ( 'NONE',  ( 1.832324720607670709, 1.448415597588696313, 0.06912397827687367935 ) ) ;
#6255 = CALENDAR_DATE ( 2026, 9, 10 ) ;
#6256 = CARTESIAN_POINT ( 'NONE',  ( 0.000000000000000000, 0.000000000000000000, 0.000000000000000000 ) ) ;
#6257 = EDGE_CURVE ( 'NONE', #5116, #340, #3605, .T. ) ;
#6258 = DIRECTION ( 'NONE',  ( 0.6157549048526804736, -0.7879377495398138809, 0.000000000000000000 ) ) ;
#6259 = ORIENTED_EDGE ( 'NONE', *, *, #3038, .T. ) ;
#6260 = VECTOR ( 'NONE', #6770, 39.37007874015748143 ) ;
#6261 = EDGE_LOOP ( 'NONE', ( #6576, #4691 ) ) ;
#6262 = CC_DESIGN_PERSON_AND_ORGANIZATION_ASSIGNMENT ( #7305, #7258, ( #7483 ) ) ;
#6263 = FACE_OUTER_BOUND ( 'NONE', #7714, .T. ) ;
#6264 = CARTESIAN_POINT ( 'NONE',  ( 0.000000000000000000, 0.6250000000000000000, 0.000000000000000000 ) ) ;
#6266 = CARTESIAN_POINT ( 'NONE',  ( 1.605841161801687900, 0.8785330470578376350, -0.1039999999999998287 ) ) ;
#6265 = CIRCLE ( 'NONE', #4554, 0.01652128394798136474 ) ;
#6267 = APPROVAL_DATE_TIME ( #4946, #2381 ) ;
#6268 = DIRECTION ( 'NONE',  ( -0.000000000000000000, -0.000000000000000000, -1.000000000000000000 ) ) ;
#6269 = AXIS2_PLACEMENT_3D ( 'NONE', #7498, #530, #5496 ) ;
#6270 = CARTESIAN_POINT ( 'NONE',  ( 6.068104892000602213, -0.009251957739379222667, 0.1849999999999999978 ) ) ;
#6271 = VERTEX_POINT ( 'NONE', #4333 ) ;
#6272 = EDGE_LOOP ( 'NONE', ( #3954, #5335, #3115, #5623 ) ) ;
#6273 = VERTEX_POINT ( 'NONE', #6110 ) ;
#6274 = CARTESIAN_POINT ( 'NONE',  ( 1.492904096916551460, 1.856349440303736831, -0.001813861035895662039 ) ) ;
#6275 = LINE ( 'NONE', #3881, #6633 ) ;
#6276 = DIRECTION ( 'NONE',  ( 0.7879377495398124376, 0.6157549048526823610, -1.469929246256068058E-15 ) ) ;
#6277 = ORIENTED_EDGE ( 'NONE', *, *, #4389, .T. ) ;
#6278 = CARTESIAN_POINT ( 'NONE',  ( 0.1250000000000000278, 0.03125000000000000000, 0.06250000000000000000 ) ) ;
#6279 = ORIENTED_EDGE ( 'NONE', *, *, #6807, .F. ) ;
#6280 = CARTESIAN_POINT ( 'NONE',  ( 0.1000000000000000472, -0.03125000000000000000, 0.7124999999999989120 ) ) ;
#6281 = CARTESIAN_POINT ( 'NONE',  ( 4.390472339057043705, -2.510390028880329805, 0.09374999999999998612 ) ) ;
#6282 = PERSON_AND_ORGANIZATION ( #4735, #6190 ) ;
#6283 = ORIENTED_EDGE ( 'NONE', *, *, #1577, .T. ) ;
#6284 = CARTESIAN_POINT ( 'NONE',  ( 1.260018307975525387, 1.633742302984368733, 0.2500000000000000000 ) ) ;
#6285 = MANIFOLD_SOLID_BREP ( 'Cut-Extrude1', #6089 ) ;
#6286 = DIRECTION ( 'NONE',  ( -1.000000000000000000, 0.000000000000000000, 0.000000000000000000 ) ) ;
#6287 = ORIENTED_EDGE ( 'NONE', *, *, #2533, .T. ) ;
#6288 = DIRECTION ( 'NONE',  ( 0.000000000000000000, -0.000000000000000000, -1.000000000000000000 ) ) ;
#6289 = CARTESIAN_POINT ( 'NONE',  ( -0.06999999999999996503, 0.03125000000000000000, 0.8125000000000000000 ) ) ;
#6290 = DIRECTION ( 'NONE',  ( 8.427892622575437673E-16, 1.361214915566403104E-15, -1.000000000000000000 ) ) ;
#6291 = FACE_OUTER_BOUND ( 'NONE', #3383, .T. ) ;
#6292 = SECURITY_CLASSIFICATION_LEVEL ( 'unclassified' ) ;
#6293 = CARTESIAN_POINT ( 'NONE',  ( 6.190219624525621356, 0.4584813330253886265, -0.1849999999999999978 ) ) ;
#6294 = ORIENTED_EDGE ( 'NONE', *, *, #5844, .T. ) ;
#6295 = ORIENTED_EDGE ( 'NONE', *, *, #1316, .T. ) ;
#6296 = CARTESIAN_POINT ( 'NONE',  ( -0.1250000000000000000, 0.5625000000000000000, 0.03125000000000000000 ) ) ;
#6297 = DIRECTION ( 'NONE',  ( 0.7879377495398135478, 0.6157549048526808066, 5.326735490302674370E-15 ) ) ;
#6298 = EDGE_CURVE ( 'NONE', #2552, #7593, #6253, .T. ) ;
#6299 = CARTESIAN_POINT ( 'NONE',  ( 0.1028096983035134554, -0.4582465879184299817, 0.03120238169111335530 ) ) ;
#6300 = PERSON_AND_ORGANIZATION ( #4735, #6190 ) ;
#6301 = DIRECTION ( 'NONE',  ( 0.8875604078987033851, -0.4606913525677331367, 0.000000000000000000 ) ) ;
#6302 = CARTESIAN_POINT ( 'NONE',  ( -0.04782642554762441683, -0.03125000000000000000, 0.07449999999999999678 ) ) ;
#6303 = ADVANCED_FACE ( 'NONE', ( #1752 ), #3670, .T. ) ;
#6304 = PRODUCT_RELATED_PRODUCT_CATEGORY ( 'detail', '', ( #7672 ) ) ;
#6305 = ADVANCED_FACE ( 'NONE', ( #6420 ), #4576, .T. ) ;
#6306 = CARTESIAN_POINT ( 'NONE',  ( 0.000000000000000000, 0.000000000000000000, 0.000000000000000000 ) ) ;
#6307 = EDGE_LOOP ( 'NONE', ( #4732, #3111, #2485, #7881, #2804, #4006 ) ) ;
#6308 = DIRECTION ( 'NONE',  ( 0.2323175946639494671, -0.9726399823210830631, 0.000000000000000000 ) ) ;
#6309 = CARTESIAN_POINT ( 'NONE',  ( 1.362414746624861506, 1.071731237471605480, -0.1509691161079382282 ) ) ;
#6310 = CARTESIAN_POINT ( 'NONE',  ( -0.02822771919328412663, 0.03615965030273324970, -0.1250000000000000000 ) ) ;
#6311 = VERTEX_POINT ( 'NONE', #5809 ) ;
#6312 = LINE ( 'NONE', #4993, #560 ) ;
#6313 = VERTEX_POINT ( 'NONE', #1918 ) ;
#6314 = CC_DESIGN_SECURITY_CLASSIFICATION ( #3550, ( #7483 ) ) ;
#6315 = CARTESIAN_POINT ( 'NONE',  ( 0.1250000000000000000, 0.000000000000000000, -0.5599999999999999423 ) ) ;
#6316 = APPROVAL_ROLE ( '' ) ;
#6317 = ORIENTED_EDGE ( 'NONE', *, *, #1171, .T. ) ;
#6318 = CARTESIAN_POINT ( 'NONE',  ( 1.272185993414492122, 1.083697202197649423, -0.08467303850119081710 ) ) ;
#6319 = DIRECTION ( 'NONE',  ( -1.000000000000000000, 0.000000000000000000, 0.000000000000000000 ) ) ;
#6320 = DIRECTION ( 'NONE',  ( 0.000000000000000000, -1.000000000000000000, 0.000000000000000000 ) ) ;
#6321 = AXIS2_PLACEMENT_3D ( 'NONE', #5627, #1813, #3662 ) ;
#6322 = CARTESIAN_POINT ( 'NONE',  ( 1.762749485016304574, 1.395289003792431037, 0.1650921806306561712 ) ) ;
#6323 = CARTESIAN_POINT ( 'NONE',  ( 1.275565605498405253, -0.08258253728086821510, -0.1849999999999999978 ) ) ;
#6324 = CARTESIAN_POINT ( 'NONE',  ( 1.524344036321053197, 1.862279377486306231, -0.0001440199302405391986 ) ) ;
#6325 = AXIS2_PLACEMENT_3D ( 'NONE', #561, #3067, #1758 ) ;
#6326 = VERTEX_POINT ( 'NONE', #4428 ) ;
#6327 = ORIENTED_EDGE ( 'NONE', *, *, #336, .F. ) ;
#6328 = EDGE_CURVE ( 'NONE', #5902, #1252, #484, .T. ) ;
#6329 = VECTOR ( 'NONE', #6814, 39.37007874015748143 ) ;
#6330 = DIRECTION ( 'NONE',  ( -0.6568496200222107007, -0.7540216022612863389, 0.000000000000000000 ) ) ;
#6331 = APPROVAL_STATUS ( 'not_yet_approved' ) ;
#6332 = DIRECTION ( 'NONE',  ( -0.000000000000000000, 0.000000000000000000, -1.000000000000000000 ) ) ;
#6333 = CARTESIAN_POINT ( 'NONE',  ( 1.780616048947831986, 1.055727875058976917, -0.1039999999999998703 ) ) ;
#6334 = ORIENTED_EDGE ( 'NONE', *, *, #7261, .F. ) ;
#6335 = ORIENTED_EDGE ( 'NONE', *, *, #3991, .F. ) ;
#6336 = AXIS2_PLACEMENT_3D ( 'NONE', #3721, #7570, #603 ) ;
#6337 = EDGE_CURVE ( 'NONE', #846, #2089, #801, .T. ) ;
#6338 = CIRCLE ( 'NONE', #6731, 0.1000000000000000194 ) ;
#6339 = ORIENTED_EDGE ( 'NONE', *, *, #6191, .F. ) ;
#6340 = MANIFOLD_SOLID_BREP ( 'Cut-Extrude5', #4783 ) ;
#6341 = CARTESIAN_POINT ( 'NONE',  ( 0.000000000000000000, 0.000000000000000000, -0.6219999999999999973 ) ) ;
#6342 = VERTEX_POINT ( 'NONE', #4460 ) ;
#6343 = DIRECTION ( 'NONE',  ( 0.7879377495398223186, 0.6157549048526698154, -0.000000000000000000 ) ) ;
#6344 = CARTESIAN_POINT ( 'NONE',  ( -1.432604426929670938, 0.8194101287839820058, -0.1250000000000000000 ) ) ;
#6345 = CC_DESIGN_SECURITY_CLASSIFICATION ( #1105, ( #8097 ) ) ;
#6346 = AXIS2_PLACEMENT_3D ( 'NONE', #7056, #3172, #6534 ) ;
#6347 = B_SPLINE_CURVE_WITH_KNOTS ( 'NONE', 3,
 ( #5713, #2500, #5010, #1280 ),
 .UNSPECIFIED., .F., .F.,
 ( 4, 4 ),
 ( 1.268750569348874822E-13, 0.0003138637853426452448 ),
 .UNSPECIFIED. ) ;
#6348 = EDGE_CURVE ( 'NONE', #7740, #2606, #2052, .T. ) ;
#6349 = CYLINDRICAL_SURFACE ( 'NONE', #25, 0.1250000000000000000 ) ;
#6350 = CARTESIAN_POINT ( 'NONE',  ( -0.1250000000000000000, 0.5625000000000000000, 0.03125000000000000000 ) ) ;
#6351 = VECTOR ( 'NONE', #3521, 39.37007874015748143 ) ;
#6352 = CARTESIAN_POINT ( 'NONE',  ( 2.013013176098461537E-17, 1.425000000000000044, -0.1487499999999999933 ) ) ;
#6353 = CARTESIAN_POINT ( 'NONE',  ( 1.101712734285305473, 0.9160746524681562253, -0.3750000000000000555 ) ) ;
#6354 = COORDINATED_UNIVERSAL_TIME_OFFSET ( 0, 0, .AHEAD. ) ;
#6355 = ORIENTED_EDGE ( 'NONE', *, *, #6048, .T. ) ;
#6356 = CARTESIAN_POINT ( 'NONE',  ( 0.000000000000000000, 0.000000000000000000, 0.06199999999999999956 ) ) ;
#6357 = CARTESIAN_POINT ( 'NONE',  ( 3.666415866878781848, -8.185094079965441694, -0.1849999999999999978 ) ) ;
#6358 = AXIS2_PLACEMENT_3D ( 'NONE', #7391, #1817, #4363 ) ;
#6359 = CARTESIAN_POINT ( 'NONE',  ( 1.258616367985684104, -0.02482036785324303815, -0.1849999999999999978 ) ) ;
#6360 = AXIS2_PLACEMENT_3D ( 'NONE', #1642, #2751, #2873 ) ;
#6361 = LINE ( 'NONE', #7621, #6634 ) ;
#6362 = CYLINDRICAL_SURFACE ( 'NONE', #3987, 0.1100000000000000006 ) ;
#6363 = DIRECTION ( 'NONE',  ( 0.000000000000000000, 1.000000000000000000, 0.000000000000000000 ) ) ;
#6364 = CARTESIAN_POINT ( 'NONE',  ( 1.713931971700676904, 1.282147506509141444, 0.1862199900718168877 ) ) ;
#6365 = AXIS2_PLACEMENT_3D ( 'NONE', #5408, #7369, #3686 ) ;
#6366 = AXIS2_PLACEMENT_3D ( 'NONE', #1959, #4465, #2045 ) ;
#6367 = VECTOR ( 'NONE', #7386, 39.37007874015748854 ) ;
#6368 = ORIENTED_EDGE ( 'NONE', *, *, #829, .F. ) ;
#6369 = LINE ( 'NONE', #756, #6776 ) ;
#6370 = SECURITY_CLASSIFICATION_LEVEL ( 'unclassified' ) ;
#6371 = DIRECTION ( 'NONE',  ( -1.000000000000000000, 0.000000000000000000, 0.000000000000000000 ) ) ;
#6372 = DIRECTION ( 'NONE',  ( 0.7879377495398141029, 0.6157549048526802515, 0.000000000000000000 ) ) ;
#6373 = ORIENTED_EDGE ( 'NONE', *, *, #2524, .F. ) ;
#6374 = AXIS2_PLACEMENT_3D ( 'NONE', #1826, #3677, #5608 ) ;
#6375 = AXIS2_PLACEMENT_3D ( 'NONE', #6264, #4861, #4324 ) ;
#6376 = EDGE_LOOP ( 'NONE', ( #2770, #3008, #5754 ) ) ;
#6377 = CIRCLE ( 'NONE', #5070, 0.2499962251234248700 ) ;
#6378 = ORIENTED_EDGE ( 'NONE', *, *, #5634, .F. ) ;
#6379 = AXIS2_PLACEMENT_3D ( 'NONE', #834, #218, #1973 ) ;
#6380 = PLANE ( 'NONE',  #4381 ) ;
#6381 = EDGE_LOOP ( 'NONE', ( #764, #7967 ) ) ;
#6382 = DIRECTION ( 'NONE',  ( 0.000000000000000000, 0.000000000000000000, 1.000000000000000000 ) ) ;
#6383 = DIRECTION ( 'NONE',  ( 0.000000000000000000, -1.000000000000000000, 0.000000000000000000 ) ) ;
#6384 = DIRECTION ( 'NONE',  ( 0.4606913525677329146, 0.8875604078987036072, -0.000000000000000000 ) ) ;
#6385 = VERTEX_POINT ( 'NONE', #6344 ) ;
#6386 = PLANE ( 'NONE',  #4757 ) ;
#6387 = ORIENTED_EDGE ( 'NONE', *, *, #6094, .F. ) ;
#6388 = CARTESIAN_POINT ( 'NONE',  ( 1.851982333143841197, 1.496483025098417796, -0.007738958973838943288 ) ) ;
#6389 = DIRECTION ( 'NONE',  ( 0.6568496200222107007, 0.7540216022612862279, -0.000000000000000000 ) ) ;
#6390 = PERSON_AND_ORGANIZATION ( #4735, #6190 ) ;
#6391 = EDGE_CURVE ( 'NONE', #7457, #6217, #186, .T. ) ;
#6392 = VERTEX_POINT ( 'NONE', #1989 ) ;
#6393 = EDGE_CURVE ( 'NONE', #7842, #3224, #6275, .T. ) ;
#6394 = FACE_OUTER_BOUND ( 'NONE', #1823, .T. ) ;
#6395 = DIRECTION ( 'NONE',  ( 1.000000000000000000, 0.000000000000000000, -1.224646799147353207E-16 ) ) ;
#6396 = ORIENTED_EDGE ( 'NONE', *, *, #2521, .F. ) ;
#6397 = EDGE_CURVE ( 'NONE', #5921, #5439, #3186, .T. ) ;
#6398 = DIRECTION ( 'NONE',  ( 1.000000000000000000, 0.000000000000000000, 0.000000000000000000 ) ) ;
#6399 = CC_DESIGN_PERSON_AND_ORGANIZATION_ASSIGNMENT ( #4168, #7706, ( #7217 ) ) ;
#6400 = ADVANCED_FACE ( 'NONE', ( #3151 ), #67, .T. ) ;
#6401 = DIRECTION ( 'NONE',  ( 0.000000000000000000, -1.000000000000000000, 0.000000000000000000 ) ) ;
#6402 = PERSON_AND_ORGANIZATION ( #4735, #6190 ) ;
#6403 = CARTESIAN_POINT ( 'NONE',  ( 0.2935750530104211387, 0.05119392622207447063, 0.07449999999999999678 ) ) ;
#6404 = PERSON_AND_ORGANIZATION_ROLE ( 'classification_officer' ) ;
#6405 = DIRECTION ( 'NONE',  ( 0.000000000000000000, 0.000000000000000000, 1.000000000000000000 ) ) ;
#6406 = ORIENTED_EDGE ( 'NONE', *, *, #168, .F. ) ;
#6407 = CARTESIAN_POINT ( 'NONE',  ( 1.693178775325104191, 1.269413987854449255, 0.1923610198617223266 ) ) ;
#6408 = ORIENTED_EDGE ( 'NONE', *, *, #1924, .T. ) ;
#6409 = ORIENTED_EDGE ( 'NONE', *, *, #4953, .F. ) ;
#6410 = CARTESIAN_POINT ( 'NONE',  ( 1.640223930642815242, 1.235377681955144746, -0.1039999999999998703 ) ) ;
#6411 = DIRECTION ( 'NONE',  ( -0.000000000000000000, -0.000000000000000000, -1.000000000000000000 ) ) ;
#6412 = CALENDAR_DATE ( 2026, 9, 10 ) ;
#6413 = PLANE ( 'NONE',  #4548 ) ;
#6414 = CARTESIAN_POINT ( 'NONE',  ( -0.1250000000000000000, 0.6250000000000000000, -0.03125000000000000000 ) ) ;
#6415 = EDGE_LOOP ( 'NONE', ( #943, #4100, #6317, #7626, #6498, #1667, #1956, #5049 ) ) ;
#6416 = EDGE_LOOP ( 'NONE', ( #4697, #4386, #5777, #5648 ) ) ;
#6417 = DIRECTION ( 'NONE',  ( -0.000000000000000000, -0.000000000000000000, 1.000000000000000000 ) ) ;
#6418 = ORIENTED_EDGE ( 'NONE', *, *, #438, .T. ) ;
#6419 = CARTESIAN_POINT ( 'NONE',  ( -0.5950975756886834889, 0.1840126700235211188, 0.2179999999999999993 ) ) ;
#6420 = FACE_OUTER_BOUND ( 'NONE', #6065, .T. ) ;
#6421 = DIRECTION ( 'NONE',  ( -0.000000000000000000, -0.000000000000000000, 1.000000000000000000 ) ) ;
#6422 = FACE_OUTER_BOUND ( 'NONE', #6673, .T. ) ;
#6423 = EDGE_CURVE ( 'NONE', #1200, #7690, #5460, .T. ) ;
#6424 = EDGE_CURVE ( 'NONE', #1428, #4761, #3888, .T. ) ;
#6425 = ORIENTED_EDGE ( 'NONE', *, *, #1319, .F. ) ;
#6426 = CARTESIAN_POINT ( 'NONE',  ( 1.846917295141469628, 1.491596352740438336, 0.01361236970061216640 ) ) ;
#6427 = DIRECTION ( 'NONE',  ( 0.000000000000000000, 0.000000000000000000, 1.000000000000000000 ) ) ;
#6428 = CALENDAR_DATE ( 2026, 9, 10 ) ;
#6429 = VERTEX_POINT ( 'NONE', #3921 ) ;
#6430 = CARTESIAN_POINT ( 'NONE',  ( 1.279420049761111233, 1.085869607567433892, -0.09058840186730054977 ) ) ;
#6431 = PLANE ( 'NONE',  #6761 ) ;
#6432 = ORIENTED_EDGE ( 'NONE', *, *, #2028, .F. ) ;
#6433 = CARTESIAN_POINT ( 'NONE',  ( -1.855136387357835481, 0.9645206712600612464, -0.08100000000000007194 ) ) ;
#6434 = EDGE_CURVE ( 'NONE', #2029, #7766, #3106, .T. ) ;
#6435 = DIRECTION ( 'NONE',  ( 0.000000000000000000, 1.000000000000000000, 0.000000000000000000 ) ) ;
#6436 = SHAPE_REPRESENTATION ( 'Cleco, Fastener, Pusher', ( #3555 ), #2771 ) ;
#6437 = DIRECTION ( 'NONE',  ( 1.000000000000000000, 0.000000000000000000, 0.000000000000000000 ) ) ;
#6438 = PERSON_AND_ORGANIZATION ( #4735, #6190 ) ;
#6439 = ORIENTED_EDGE ( 'NONE', *, *, #7741, .T. ) ;
#6440 = ORIENTED_EDGE ( 'NONE', *, *, #7831, .T. ) ;
#6441 = DIRECTION ( 'NONE',  ( -1.000000000000000000, 0.000000000000000000, 0.000000000000000000 ) ) ;
#6442 = EDGE_CURVE ( 'NONE', #1018, #4570, #3229, .T. ) ;
#6443 = CARTESIAN_POINT ( 'NONE',  ( 1.417311200634858492, 1.162707465448240773, 0.2206888379057397043 ) ) ;
#6444 = LOCAL_TIME ( 14, 45, 32.00000000000000000, #1683 ) ;
#6445 = MANIFOLD_SOLID_BREP ( 'Fillet8', #7652 ) ;
#6446 = AXIS2_PLACEMENT_3D ( 'NONE', #2643, #5897, #2037 ) ;
#6447 = ORIENTED_EDGE ( 'NONE', *, *, #378, .T. ) ;
#6448 = CC_DESIGN_APPROVAL ( #5598, ( #4611 ) ) ;
#6449 = LINE ( 'NONE', #5757, #4475 ) ;
#6450 = EDGE_LOOP ( 'NONE', ( #3095, #1042, #264, #6207 ) ) ;
#6451 = LINE ( 'NONE', #791, #3063 ) ;
#6452 = COORDINATED_UNIVERSAL_TIME_OFFSET ( 0, 0, .AHEAD. ) ;
#6453 = CARTESIAN_POINT ( 'NONE',  ( 0.000000000000000000, 0.6250000000000000000, 0.000000000000000000 ) ) ;
#6454 = LINE ( 'NONE', #1947, #60 ) ;
#6455 = VECTOR ( 'NONE', #5375, 39.37007874015748143 ) ;
#6456 = ORIENTED_EDGE ( 'NONE', *, *, #7091, .T. ) ;
#6457 = EDGE_CURVE ( 'NONE', #7619, #7457, #7675, .T. ) ;
#6458 = EDGE_LOOP ( 'NONE', ( #8065, #1409, #4071, #901, #1498 ) ) ;
#6459 = VERTEX_POINT ( 'NONE', #1416 ) ;
#6460 = VECTOR ( 'NONE', #5937, 39.37007874015748143 ) ;
#6461 = ORIENTED_EDGE ( 'NONE', *, *, #1458, .F. ) ;
#6462 = CYLINDRICAL_SURFACE ( 'NONE', #5553, 0.1204106507132265275 ) ;
#6463 = ORIENTED_EDGE ( 'NONE', *, *, #6595, .T. ) ;
#6464 = ORIENTED_EDGE ( 'NONE', *, *, #6193, .T. ) ;
#6465 = LINE ( 'NONE', #5808, #7254 ) ;
#6466 = FACE_OUTER_BOUND ( 'NONE', #3826, .T. ) ;
#6467 = DIRECTION ( 'NONE',  ( -0.9987955914953421388, -0.04906492035527518225, 0.000000000000000000 ) ) ;
#6468 = VECTOR ( 'NONE', #6874, 39.37007874015748143 ) ;
#6469 = ORIENTED_EDGE ( 'NONE', *, *, #5838, .F. ) ;
#6470 = CIRCLE ( 'NONE', #4110, 0.09507037842118626347 ) ;
#6471 = DIRECTION ( 'NONE',  ( -0.6157549048526802515, 0.7879377495398142139, -0.000000000000000000 ) ) ;
#6472 = AXIS2_PLACEMENT_3D ( 'NONE', #5063, #6947, #7680 ) ;
#6473 = CC_DESIGN_SECURITY_CLASSIFICATION ( #448, ( #8095 ) ) ;
#6474 = CARTESIAN_POINT ( 'NONE',  ( 1.797977497908697764, 1.451469997631733344, 0.1179144137747096116 ) ) ;
#6475 = CARTESIAN_POINT ( 'NONE',  ( -0.04782642554762442377, -0.07812500000000000000, 0.07449999999999999678 ) ) ;
#6476 = PERSON_AND_ORGANIZATION ( #4735, #6190 ) ;
#6477 = ORIENTED_EDGE ( 'NONE', *, *, #74, .F. ) ;
#6478 = CARTESIAN_POINT ( 'NONE',  ( 3.666415866878781848, -8.185094079965441694, -0.1250000000000000000 ) ) ;
#6479 = CARTESIAN_POINT ( 'NONE',  ( 0.3426393240825695297, -0.3526608655151391991, 0.01152805889772838717 ) ) ;
#6480 = ORIENTED_EDGE ( 'NONE', *, *, #1330, .F. ) ;
#6481 = DIRECTION ( 'NONE',  ( -0.9726399823210830631, -0.2323175946639496336, -0.000000000000000000 ) ) ;
#6482 = AXIS2_PLACEMENT_3D ( 'NONE', #7517, #2094, #4032 ) ;
#6483 = DIRECTION ( 'NONE',  ( 0.000000000000000000, 0.000000000000000000, 1.000000000000000000 ) ) ;
#6484 = DIRECTION ( 'NONE',  ( -0.000000000000000000, -1.000000000000000000, -0.000000000000000000 ) ) ;
#6485 = AXIS2_PLACEMENT_3D ( 'NONE', #5272, #4726, #4821 ) ;
#6486 = DATE_AND_TIME ( #5378, #6061 ) ;
#6487 = VERTEX_POINT ( 'NONE', #3962 ) ;
#6488 = TOROIDAL_SURFACE ( 'NONE', #2950, 6.962657474112426748, 0.03200000000000000067 ) ;
#6489 = ADVANCED_FACE ( 'NONE', ( #6466 ), #7121, .F. ) ;
#6490 = LINE ( 'NONE', #876, #7275 ) ;
#6491 = EDGE_CURVE ( 'NONE', #4303, #7230, #879, .T. ) ;
#6492 = EDGE_CURVE ( 'NONE', #5845, #4303, #4940, .T. ) ;
#6493 = CARTESIAN_POINT ( 'NONE',  ( 1.655938099986013379, 1.304250990722249037, 0.1968515939248739743 ) ) ;
#6494 = EDGE_CURVE ( 'NONE', #7764, #4881, #7168, .T. ) ;
#6495 = AXIS2_PLACEMENT_3D ( 'NONE', #6032, #5223, #7793 ) ;
#6496 = APPROVAL ( #6768, 'UNSPECIFIED' ) ;
#6497 = ORIENTED_EDGE ( 'NONE', *, *, #7986, .F. ) ;
#6498 = ORIENTED_EDGE ( 'NONE', *, *, #3381, .F. ) ;
#6499 = EDGE_CURVE ( 'NONE', #5472, #6917, #4017, .T. ) ;
#6500 = DIRECTION ( 'NONE',  ( -0.000000000000000000, -0.000000000000000000, -1.000000000000000000 ) ) ;
#6501 = CARTESIAN_POINT ( 'NONE',  ( 0.000000000000000000, 0.000000000000000000, -0.5599999999999999423 ) ) ;
#6502 = APPROVAL_DATE_TIME ( #301, #2789 ) ;
#6503 = LINE ( 'NONE', #2257, #8062 ) ;
#6504 = LINE ( 'NONE', #7226, #1251 ) ;
#6505 = CIRCLE ( 'NONE', #7535, 0.2819999999999998619 ) ;
#6506 = EDGE_CURVE ( 'NONE', #7782, #6877, #1923, .T. ) ;
#6507 = EDGE_LOOP ( 'NONE', ( #182, #1844, #6906, #7887, #2529 ) ) ;
#6508 = AXIS2_PLACEMENT_3D ( 'NONE', #6353, #3197, #808 ) ;
#6509 = ORIENTED_EDGE ( 'NONE', *, *, #781, .T. ) ;
#6510 = VECTOR ( 'NONE', #915, 39.37007874015748143 ) ;
#6511 = PRODUCT ( 'MAS-157, Fastener', 'MAS-157, Fastener', '', ( #4998 ) ) ;
#6512 = PRODUCT_RELATED_PRODUCT_CATEGORY ( 'detail', '', ( #7217 ) ) ;
#6513 = EDGE_CURVE ( 'NONE', #7994, #7663, #2817, .T. ) ;
#6514 = ORIENTED_EDGE ( 'NONE', *, *, #5635, .T. ) ;
#6515 = ORIENTED_EDGE ( 'NONE', *, *, #3180, .F. ) ;
#6516 = DIRECTION ( 'NONE',  ( -0.000000000000000000, -0.000000000000000000, -1.000000000000000000 ) ) ;
#6517 = ORIENTED_EDGE ( 'NONE', *, *, #6181, .T. ) ;
#6518 = PERSON ( 'NAUO-PER9', 'UNSPECIFIED', 'UNSPECIFIED', ('UNSPECIFIED'), ('UNSPECIFIED'), ('UNSPECIFIED') ) ;
#6520 = CARTESIAN_POINT ( 'NONE',  ( 1.597320645397854122, 1.292162771345663375, 0.2367737893327029053 ) ) ;
#6519 = AXIS2_PLACEMENT_3D ( 'NONE', #7412, #2400, #1098 ) ;
#6521 = DIRECTION ( 'NONE',  ( -0.000000000000000000, -0.000000000000000000, -1.000000000000000000 ) ) ;
#6522 = VECTOR ( 'NONE', #3099, 39.37007874015748143 ) ;
#6523 = DIRECTION ( 'NONE',  ( 0.9987955914953421388, 0.04906492035527377366, 0.000000000000000000 ) ) ;
#6524 = DIRECTION ( 'NONE',  ( -0.000000000000000000, -0.000000000000000000, -1.000000000000000000 ) ) ;
#6525 = CIRCLE ( 'NONE', #2979, 0.2148203157102361871 ) ;
#6526 = VERTEX_POINT ( 'NONE', #2206 ) ;
#6527 = DIRECTION ( 'NONE',  ( 0.000000000000000000, -0.000000000000000000, -1.000000000000000000 ) ) ;
#6528 = DIRECTION ( 'NONE',  ( -0.9987955914953421388, -0.04906492035527377366, 0.000000000000000000 ) ) ;
#6529 = DATE_AND_TIME ( #6428, #2773 ) ;
#6530 = DIRECTION ( 'NONE',  ( 0.000000000000000000, 1.000000000000000000, -0.000000000000000000 ) ) ;
#6531 = CYLINDRICAL_SURFACE ( 'NONE', #1653, 9.064497838702109789 ) ;
#6532 = ORIENTED_EDGE ( 'NONE', *, *, #6551, .T. ) ;
#6533 = CARTESIAN_POINT ( 'NONE',  ( 1.339249842318065653, 1.071711091725345621, -0.1040000000000607383 ) ) ;
#6534 = DIRECTION ( 'NONE',  ( 1.000000000000000000, 2.841121913410833274E-14, 0.000000000000000000 ) ) ;
#6535 = LINE ( 'NONE', #1638, #5996 ) ;
#6536 = PERSON_AND_ORGANIZATION_ROLE ( 'classification_officer' ) ;
#6537 = EDGE_LOOP ( 'NONE', ( #6744, #468, #12, #2632 ) ) ;
#6538 = CYLINDRICAL_SURFACE ( 'NONE', #1644, 0.2149999999999995803 ) ;
#6539 = B_SPLINE_CURVE_WITH_KNOTS ( 'NONE', 3,
 ( #1824, #6299, #6175, #1861, #2472, #4862, #673, #5557, #8040, #5475, #1204, #1743, #4252, #4369, #592, #5640, #2436, #4945 ),
 .UNSPECIFIED., .F., .F.,
 ( 4, 2, 2, 2, 2, 2, 2, 2, 4 ),
 ( 0.000000000000000000, 5.948296474276362620E-05, 0.0001189659294855272524, 0.0002379318589710563479, 0.0004758637179421140511, 0.0009517274358842289696, 0.001903454871768459240, 0.002855182307652689294, 0.003806909743536920215 ),
 .UNSPECIFIED. ) ;
#6540 = CARTESIAN_POINT ( 'NONE',  ( 1.488944392314652365, 1.220926469523529345, 0.2500000000000000000 ) ) ;
#6541 = ORIENTED_EDGE ( 'NONE', *, *, #1668, .T. ) ;
#6542 = VERTEX_POINT ( 'NONE', #4618 ) ;
#6543 = EDGE_CURVE ( 'NONE', #4885, #1649, #233, .T. ) ;
#6544 = VERTEX_POINT ( 'NONE', #908 ) ;
#6545 = DIRECTION ( 'NONE',  ( 0.04906492035527816598, -0.9987955914953420278, 0.000000000000000000 ) ) ;
#6546 = CARTESIAN_POINT ( 'NONE',  ( 1.449725606734969752, 1.190739840093742563, 0.2500000000000000000 ) ) ;
#6547 = ITEM_DEFINED_TRANSFORMATION ( 'NONE', 'NONE', #5791,  #416 ) ;
#6548 = DIRECTION ( 'NONE',  ( 0.6157549048526802515, -0.7879377495398142139, 0.000000000000000000 ) ) ;
#6549 = VERTEX_POINT ( 'NONE', #3400 ) ;
#6550 = ORIENTED_EDGE ( 'NONE', *, *, #1731, .T. ) ;
#6551 = EDGE_CURVE ( 'NONE', #1218, #3851, #5727, .T. ) ;
#6552 = EDGE_CURVE ( 'NONE', #684, #4837, #3924, .T. ) ;
#6553 = DIRECTION ( 'NONE',  ( 0.7879377495398135478, 0.6157549048526808066, 1.794268796733532573E-15 ) ) ;
#6554 = ADVANCED_FACE ( 'NONE', ( #1583 ), #4151, .T. ) ;
#6555 = LINE ( 'NONE', #4167, #6989 ) ;
#6556 = DIRECTION ( 'NONE',  ( -0.4964005096718474008, -0.8680936205257645533, 0.000000000000000000 ) ) ;
#6557 = CARTESIAN_POINT ( 'NONE',  ( 1.472947776714219836, 0.7825821671288679671, 5.393636709996481038 ) ) ;
#6558 = ADVANCED_FACE ( 'NONE', ( #5282 ), #1552, .T. ) ;
#6559 = CARTESIAN_POINT ( 'NONE',  ( -0.03125000000000000000, 0.7500000000000001110, -0.1106726592253027691 ) ) ;
#6560 = CARTESIAN_POINT ( 'NONE',  ( 1.475891671935536609, 0.7226544316391472211, 0.09375000000000005551 ) ) ;
#6561 = CARTESIAN_POINT ( 'NONE',  ( 0.1250000000000000000, 0.6250000000000000000, -0.03125000000000000000 ) ) ;
#6562 = CARTESIAN_POINT ( 'NONE',  ( 0.3495740218478449179, -0.3469141891495676200, 0.01729592239954550956 ) ) ;
#6563 = VERTEX_POINT ( 'NONE', #7847 ) ;
#6564 = CARTESIAN_POINT ( 'NONE',  ( 3.690413561029368683, -8.374393170229348371, 0.1849999999999999978 ) ) ;
#6565 = PLANE ( 'NONE',  #582 ) ;
#6566 = APPLICATION_CONTEXT ( 'configuration controlled 3d designs of mechanical parts and assemblies' ) ;
#6567 = CARTESIAN_POINT ( 'NONE',  ( 1.515881672266826685, 1.874305877512008722, -0.03993337778610878130 ) ) ;
#6568 = APPROVAL_STATUS ( 'not_yet_approved' ) ;
#6569 = ORIENTED_EDGE ( 'NONE', *, *, #5788, .T. ) ;
#6570 = CARTESIAN_POINT ( 'NONE',  ( 0.3095788249173507256, -0.3772292882094739341, 0.2494153240220254031 ) ) ;
#6571 = LINE ( 'NONE', #1604, #961 ) ;
#6572 = EDGE_LOOP ( 'NONE', ( #6713, #7529, #7765, #1998 ) ) ;
#6573 = APPROVAL_PERSON_ORGANIZATION ( #5414, #3935, #4880 ) ;
#6574 = VERTEX_POINT ( 'NONE', #5935 ) ;
#6575 = LENGTH_MEASURE_WITH_UNIT ( LENGTH_MEASURE( 0.02539999999999999897 ), #2194 );
#6576 = ORIENTED_EDGE ( 'NONE', *, *, #7635, .F. ) ;
#6577 = CARTESIAN_POINT ( 'NONE',  ( 0.03125000000000000000, 0.7500000000000001110, 0.1106726592253027691 ) ) ;
#6578 = LOCAL_TIME ( 14, 45, 32.00000000000000000, #5209 ) ;
#6579 = APPROVAL_ROLE ( '' ) ;
#6580 = FACE_OUTER_BOUND ( 'NONE', #3116, .T. ) ;
#6581 = VECTOR ( 'NONE', #727, 39.37007874015748143 ) ;
#6582 = ORIENTED_EDGE ( 'NONE', *, *, #1537, .T. ) ;
#6583 = DIRECTION ( 'NONE',  ( 0.000000000000000000, -1.000000000000000000, 0.000000000000000000 ) ) ;
#6584 = CIRCLE ( 'NONE', #423, 0.1000000000000000472 ) ;
#6585 = LINE ( 'NONE', #7878, #4501 ) ;
#6586 = CARTESIAN_POINT ( 'NONE',  ( 0.07000000000000002054, -0.03125000000000000000, 0.8125000000000000000 ) ) ;
#6587 = ADVANCED_FACE ( 'NONE', ( #311 ), #4086, .T. ) ;
#6588 = DIRECTION ( 'NONE',  ( -1.000000000000000000, 0.000000000000000000, 0.000000000000000000 ) ) ;
#6589 = EDGE_CURVE ( 'NONE', #81, #5187, #3729, .T. ) ;
#6590 = FACE_OUTER_BOUND ( 'NONE', #7330, .T. ) ;
#6591 = AXIS2_PLACEMENT_3D ( 'NONE', #4500, #113, #693 ) ;
#6592 = PRODUCT_RELATED_PRODUCT_CATEGORY ( 'detail', '', ( #795 ) ) ;
#6593 = VERTEX_POINT ( 'NONE', #6586 ) ;
#6594 = FACE_OUTER_BOUND ( 'NONE', #1948, .T. ) ;
#6595 = EDGE_CURVE ( 'NONE', #2638, #5062, #5397, .T. ) ;
#6596 = DIRECTION ( 'NONE',  ( -0.000000000000000000, -0.000000000000000000, 1.000000000000000000 ) ) ;
#6597 = AXIS2_PLACEMENT_3D ( 'NONE', #3538, #217, #5227 ) ;
#6598 = CARTESIAN_POINT ( 'NONE',  ( 0.8923633780935229520, 0.7607014108325300672, 0.2500000000000000000 ) ) ;
#6599 = ORIENTED_EDGE ( 'NONE', *, *, #1328, .T. ) ;
#6600 = EDGE_CURVE ( 'NONE', #1252, #353, #3592, .T. ) ;
#6601 = FACE_OUTER_BOUND ( 'NONE', #285, .T. ) ;
#6602 = TOROIDAL_SURFACE ( 'NONE', #4768, 0.4024878104020024328, 0.1000000000000000056 ) ;
#6603 = CIRCLE ( 'NONE', #3598, 0.1255000000000000282 ) ;
#6604 = DIRECTION ( 'NONE',  ( 1.000000000000000000, 0.000000000000000000, 0.000000000000000000 ) ) ;
#6605 = CARTESIAN_POINT ( 'NONE',  ( 1.490941149118869546, 1.854815442554424543, -0.04324422884743918394 ) ) ;
#6606 = DATE_TIME_ROLE ( 'classification_date' ) ;
#6607 = ORIENTED_EDGE ( 'NONE', *, *, #7047, .F. ) ;
#6608 = CARTESIAN_POINT ( 'NONE',  ( 0.2976660692273690456, -0.3850326757561704505, 0.2500000000000000000 ) ) ;
#6609 = AXIS2_PLACEMENT_3D ( 'NONE', #5677, #2793, #919 ) ;
#6610 = DIRECTION ( 'NONE',  ( -0.000000000000000000, -0.000000000000000000, -1.000000000000000000 ) ) ;
#6611 = VERTEX_POINT ( 'NONE', #5559 ) ;
#6612 = ORIENTED_EDGE ( 'NONE', *, *, #29, .T. ) ;
#6613 = AXIS2_PLACEMENT_3D ( 'NONE', #7239, #5436, #7083 ) ;
#6614 = VECTOR ( 'NONE', #3553, 39.37007874015748143 ) ;
#6615 = DIRECTION ( 'NONE',  ( 0.9999999999999998890, 4.406009580337756690E-13, 3.468464719177433508E-13 ) ) ;
#6616 = VERTEX_POINT ( 'NONE', #2392 ) ;
#6617 = DIRECTION ( 'NONE',  ( 0.000000000000000000, 0.000000000000000000, 1.000000000000000000 ) ) ;
#6618 = CARTESIAN_POINT ( 'NONE',  ( -1.040997396242601791, -0.7528336330030668266, 0.02354365816211315479 ) ) ;
#6619 = FACE_OUTER_BOUND ( 'NONE', #1093, .T. ) ;
#6620 = ORIENTED_EDGE ( 'NONE', *, *, #2363, .F. ) ;
#6621 = AXIS2_PLACEMENT_3D ( 'NONE', #931, #2152, #3423 ) ;
#6622 = ORIENTED_EDGE ( 'NONE', *, *, #4390, .F. ) ;
#6623 = CARTESIAN_POINT ( 'NONE',  ( 0.03125000000000000000, 0.03125000000000000000, -0.1204106507132265275 ) ) ;
#6624 = AXIS2_PLACEMENT_3D ( 'NONE', #7465, #2341, #2299 ) ;
#6625 = CYLINDRICAL_SURFACE ( 'NONE', #442, 0.1875000000000000278 ) ;
#6626 = CARTESIAN_POINT ( 'NONE',  ( 1.353790921086396093, 0.002306479836701611809, -0.1250000000000000278 ) ) ;
#6627 = LINE ( 'NONE', #2048, #5311 ) ;
#6628 = VERTEX_POINT ( 'NONE', #2978 ) ;
#6629 = CIRCLE ( 'NONE', #1916, 0.03125000000000000694 ) ;
#6630 = CARTESIAN_POINT ( 'NONE',  ( -1.424379639128854791, 0.8545203780043559849, -0.1657613293278376587 ) ) ;
#6631 = DIRECTION ( 'NONE',  ( -0.000000000000000000, -1.000000000000000000, -0.000000000000000000 ) ) ;
#6632 = VECTOR ( 'NONE', #4137, 39.37007874015748143 ) ;
#6633 = VECTOR ( 'NONE', #6920, 39.37007874015748143 ) ;
#6634 = VECTOR ( 'NONE', #746, 39.37007874015748143 ) ;
#6635 = LINE ( 'NONE', #5445, #6351 ) ;
#6636 = DIRECTION ( 'NONE',  ( -0.000000000000000000, 0.000000000000000000, -1.000000000000000000 ) ) ;
#6637 = DIRECTION ( 'NONE',  ( -1.000000000000000000, 0.000000000000000000, -0.000000000000000000 ) ) ;
#6638 = VERTEX_POINT ( 'NONE', #513 ) ;
#6639 = VECTOR ( 'NONE', #6371, 39.37007874015748143 ) ;
#6640 = DIRECTION ( 'NONE',  ( -1.000000000000000000, 0.000000000000000000, 0.000000000000000000 ) ) ;
#6641 = VECTOR ( 'NONE', #6701, 39.37007874015748143 ) ;
#6642 = EDGE_CURVE ( 'NONE', #5439, #5004, #6787, .T. ) ;
#6643 = AXIS2_PLACEMENT_3D ( 'NONE', #2580, #3367, #198 ) ;
#6644 = CARTESIAN_POINT ( 'NONE',  ( -1.194903880989551359, -0.2358655892081394090, 0.000000000000000000 ) ) ;
#6645 = AXIS2_PLACEMENT_3D ( 'NONE', #5343, #4714, #6676 ) ;
#6646 = CARTESIAN_POINT ( 'NONE',  ( 1.495180927969594009, 1.858128730468791678, 0.009522852913174784106 ) ) ;
#6647 = APPROVAL_DATE_TIME ( #4148, #2132 ) ;
#6648 = EDGE_LOOP ( 'NONE', ( #3315, #3170, #121, #7806 ) ) ;
#6649 = ADVANCED_FACE ( 'NONE', ( #3055 ), #5477, .F. ) ;
#6650 = DIRECTION ( 'NONE',  ( 0.000000000000000000, 0.000000000000000000, -1.000000000000000000 ) ) ;
#6651 = CARTESIAN_POINT ( 'NONE',  ( 0.3553227796840386921, -0.3420127083024185333, 0.2250125263929970976 ) ) ;
#6652 = CARTESIAN_POINT ( 'NONE',  ( 1.459523535701868324, 1.198274184545364829, 0.2499999999999795719 ) ) ;
#6653 = CC_DESIGN_PERSON_AND_ORGANIZATION_ASSIGNMENT ( #4583, #2271, ( #7247 ) ) ;
#6654 = ADVANCED_FACE ( 'NONE', ( #4905 ), #2352, .T. ) ;
#6655 = ORIENTED_EDGE ( 'NONE', *, *, #6756, .F. ) ;
#6656 = EDGE_LOOP ( 'NONE', ( #2525, #2113, #7427, #4374, #7749, #5178, #4580, #3158, #3461, #274 ) ) ;
#6657 = CARTESIAN_POINT ( 'NONE',  ( 1.859753234433174418, 1.471617347716406288, -0.009971652696953780398 ) ) ;
#6658 = LINE ( 'NONE', #381, #2713 ) ;
#6659 = DATE_AND_TIME ( #2230, #3163 ) ;
#6660 = LINE ( 'NONE', #892, #2031 ) ;
#6661 = CARTESIAN_POINT ( 'NONE',  ( 1.640223930642815242, 1.235377681955144746, -0.1039999999999998703 ) ) ;
#6662 = DIRECTION ( 'NONE',  ( -0.6157549048526801405, 0.7879377495398141029, 0.000000000000000000 ) ) ;
#6663 = APPROVAL_ROLE ( '' ) ;
#6664 = DIRECTION ( 'NONE',  ( 0.000000000000000000, 0.000000000000000000, -1.000000000000000000 ) ) ;
#6665 = CARTESIAN_POINT ( 'NONE',  ( 1.353816004522938599, 0.002313473902802895728, -0.1250000000000000278 ) ) ;
#6666 = ORIENTED_EDGE ( 'NONE', *, *, #7351, .T. ) ;
#6667 = FACE_OUTER_BOUND ( 'NONE', #1402, .T. ) ;
#6668 = FACE_OUTER_BOUND ( 'NONE', #6904, .T. ) ;
#6669 = VERTEX_POINT ( 'NONE', #5515 ) ;
#6670 = DIRECTION ( 'NONE',  ( -1.000000000000000000, 0.000000000000000000, 0.000000000000000000 ) ) ;
#6671 = DIRECTION ( 'NONE',  ( 0.000000000000000000, 0.000000000000000000, 1.000000000000000000 ) ) ;
#6672 = DIRECTION ( 'NONE',  ( 1.000000000000000000, 3.824587191129967323E-15, 0.000000000000000000 ) ) ;
#6673 = EDGE_LOOP ( 'NONE', ( #5190, #5833, #4535, #1401 ) ) ;
#6674 = CYLINDRICAL_SURFACE ( 'NONE', #3714, 0.03200000000000008393 ) ;
#6675 = CARTESIAN_POINT ( 'NONE',  ( 1.733157827470031220, 1.373632878362992527, 0.1887011865795288901 ) ) ;
#6676 = DIRECTION ( 'NONE',  ( -1.000000000000000000, 0.000000000000000000, 0.000000000000000000 ) ) ;
#6677 = PERSON_AND_ORGANIZATION ( #4735, #6190 ) ;
#6678 = ORIENTED_EDGE ( 'NONE', *, *, #7688, .F. ) ;
#6679 = DIRECTION ( 'NONE',  ( -0.6568496200222107007, -0.7540216022612862279, 0.000000000000000000 ) ) ;
#6680 = DIRECTION ( 'NONE',  ( -0.000000000000000000, -0.000000000000000000, -1.000000000000000000 ) ) ;
#6681 = CARTESIAN_POINT ( 'NONE',  ( 0.000000000000000000, 0.000000000000000000, 0.06199999999999999956 ) ) ;
#6682 = ADVANCED_FACE ( 'NONE', ( #1703 ), #7553, .T. ) ;
#6683 = EDGE_CURVE ( 'NONE', #6593, #2684, #4209, .T. ) ;
#6684 = ADVANCED_FACE ( 'NONE', ( #3017 ), #1206, .F. ) ;
#6685 = ORIENTED_EDGE ( 'NONE', *, *, #3797, .F. ) ;
#6686 = ORIENTED_EDGE ( 'NONE', *, *, #2235, .T. ) ;
#6687 = APPROVAL ( #930, 'UNKNOWN' ) ;
#6688 = EDGE_CURVE ( 'NONE', #5803, #7906, #2571, .T. ) ;
#6689 =( NAMED_UNIT ( * ) SI_UNIT ( $, .STERADIAN. ) SOLID_ANGLE_UNIT ( ) );
#6690 = ORIENTED_EDGE ( 'NONE', *, *, #3040, .T. ) ;
#6691 = CARTESIAN_POINT ( 'NONE',  ( -0.1210307295689817542, 0.6124999999999999334, 0.03125000000000000000 ) ) ;
#6692 = CARTESIAN_POINT ( 'NONE',  ( 0.08210456126311437008, -0.4609633126210107013, 0.2297859553102247487 ) ) ;
#6693 = EDGE_CURVE ( 'NONE', #5116, #963, #1796, .T. ) ;
#6694 = DATE_AND_TIME ( #2308, #2156 ) ;
#6695 = DIRECTION ( 'NONE',  ( 1.000000000000000000, 0.000000000000000000, 0.000000000000000000 ) ) ;
#6696 = SECURITY_CLASSIFICATION ( '', '', #6370 ) ;
#6697 = EDGE_CURVE ( 'NONE', #1984, #19, #2844, .T. ) ;
#6698 = VERTEX_POINT ( 'NONE', #1787 ) ;
#6699 = LOCAL_TIME ( 14, 45, 32.00000000000000000, #6927 ) ;
#6700 = CARTESIAN_POINT ( 'NONE',  ( 1.278468178840724834, 1.054204894366048473, -0.03540237177934978802 ) ) ;
#6701 = DIRECTION ( 'NONE',  ( -1.000000000000000000, 0.000000000000000000, 0.000000000000000000 ) ) ;
#6702 = DIRECTION ( 'NONE',  ( 0.000000000000000000, 1.000000000000000000, 0.000000000000000000 ) ) ;
#6703 =( BOUNDED_SURFACE ( )  B_SPLINE_SURFACE ( 3, 2, ( 
 ( #3961, #725, #6955 ),
 ( #5239, #4016, #7604 ),
 ( #6520, #765, #185 ),
 ( #2685, #2767, #3306 ),
 ( #7074, #4541, #5197 ),
 ( #907, #5766, #3399 ),
 ( #2731, #3920, #7696 ),
 ( #5281, #4459, #1334 ),
 ( #2076, #1502, #4575 ),
 ( #1453, #3228, #2114 ),
 ( #849, #3842, #3355 ),
 ( #5855, #232, #5893 ) ),
 .UNSPECIFIED., .F., .F., .T. ) 
 B_SPLINE_SURFACE_WITH_KNOTS ( ( 4, 2, 2, 2, 2, 4 ),
 ( 3, 3 ),
 ( 0.000000000000000000, 0.001189084327048017331, 0.002378168654096034663, 0.003567252981144052211, 0.004161795144668060768, 0.004756337308192069326 ),
 ( 0.000000000000000000, 1.000000000000000000 ),
 .UNSPECIFIED. ) 
 GEOMETRIC_REPRESENTATION_ITEM ( )  RATIONAL_B_SPLINE_SURFACE ( (
 ( 1.000000000000000000, 0.8944458564818607016, 1.000000000000000000),
 ( 1.000000000000000000, 0.8965647441026000086, 1.000000000000000000),
 ( 1.000000000000000000, 0.8984366196282288497, 1.000000000000000000),
 ( 1.000000000000000000, 0.9019236665693611821, 1.000000000000000000),
 ( 1.000000000000000000, 0.9035407145860101519, 1.000000000000000000),
 ( 1.000000000000000000, 0.9068047609391414188, 1.000000000000000000),
 ( 1.000000000000000000, 0.9084452571090311235, 1.000000000000000000),
 ( 1.000000000000000000, 0.9110247302869100006, 1.000000000000000000),
 ( 1.000000000000000000, 0.9119054567922144638, 1.000000000000000000),
 ( 1.000000000000000000, 0.9137037716224694073, 1.000000000000000000),
 ( 1.000000000000000000, 0.9146239968701178613, 1.000000000000000000),
 ( 1.000000000000000000, 0.9155198504394047587, 1.000000000000000000) ) ) 
 REPRESENTATION_ITEM ( '' )  SURFACE ( )  );
#6704 = DATE_TIME_ROLE ( 'creation_date' ) ;
#6705 = CYLINDRICAL_SURFACE ( 'NONE', #4290, 0.1250000000000000000 ) ;
#6706 = ORIENTED_EDGE ( 'NONE', *, *, #5028, .F. ) ;
#6707 = CIRCLE ( 'NONE', #3169, 0.2923589946935200579 ) ;
#6708 = ORIENTED_EDGE ( 'NONE', *, *, #2372, .F. ) ;
#6709 = CARTESIAN_POINT ( 'NONE',  ( 1.558885140107740819, 1.229058585821087179, 0.1943387615105033328 ) ) ;
#6710 = DIRECTION ( 'NONE',  ( -1.000000000000000000, 0.000000000000000000, 0.000000000000000000 ) ) ;
#6711 = APPROVAL_PERSON_ORGANIZATION ( #102, #4742, #176 ) ;
#6712 = CIRCLE ( 'NONE', #7103, 8.573908398499121120 ) ;
#6713 = ORIENTED_EDGE ( 'NONE', *, *, #4685, .F. ) ;
#6714 = CC_DESIGN_SECURITY_CLASSIFICATION ( #5404, ( #7756 ) ) ;
#6715 = DIRECTION ( 'NONE',  ( 1.000000000000000000, 0.000000000000000000, 0.000000000000000000 ) ) ;
#6716 = DIRECTION ( 'NONE',  ( 0.7879377495398138809, 0.6157549048526804736, 0.000000000000000000 ) ) ;
#6717 = DIRECTION ( 'NONE',  ( 1.000000000000000000, 0.000000000000000000, 0.000000000000000000 ) ) ;
#6718 = ORIENTED_EDGE ( 'NONE', *, *, #1724, .T. ) ;
#6719 = AXIS2_PLACEMENT_3D ( 'NONE', #7253, #1028, #1560 ) ;
#6720 = VERTEX_POINT ( 'NONE', #1168 ) ;
#6721 = CARTESIAN_POINT ( 'NONE',  ( 1.562204911103271421, 1.174407644688458818, 0.1842828921574816425 ) ) ;
#6722 = TOROIDAL_SURFACE ( 'NONE', #7115, 0.1487499999999999933, 0.03125000000000000000 ) ;
#6723 = DIRECTION ( 'NONE',  ( -0.000000000000000000, -0.000000000000000000, -1.000000000000000000 ) ) ;
#6724 = DIRECTION ( 'NONE',  ( -1.000000000000000000, 0.000000000000000000, 0.000000000000000000 ) ) ;
#6725 = APPROVAL_STATUS ( 'not_yet_approved' ) ;
#6726 = ORIENTED_EDGE ( 'NONE', *, *, #6492, .F. ) ;
#6727 = CARTESIAN_POINT ( 'NONE',  ( 0.000000000000000000, 0.000000000000000000, 0.000000000000000000 ) ) ;
#6728 = DIRECTION ( 'NONE',  ( -1.000000000000000000, 0.000000000000000000, 0.000000000000000000 ) ) ;
#6729 = LINE ( 'NONE', #6773, #5008 ) ;
#6730 = CIRCLE ( 'NONE', #5022, 0.1799999999999999933 ) ;
#6731 = AXIS2_PLACEMENT_3D ( 'NONE', #4516, #7017, #5685 ) ;
#6732 = ORIENTED_EDGE ( 'NONE', *, *, #8081, .F. ) ;
#6733 = APPROVAL_PERSON_ORGANIZATION ( #540, #1233, #1161 ) ;
#6734 =( NAMED_UNIT ( * ) SI_UNIT ( $, .STERADIAN. ) SOLID_ANGLE_UNIT ( ) );
#6735 = ORIENTED_EDGE ( 'NONE', *, *, #1578, .F. ) ;
#6736 = ADVANCED_FACE ( 'NONE', ( #3545 ), #4327, .F. ) ;
#6737 = DIRECTION ( 'NONE',  ( 0.000000000000000000, 0.000000000000000000, 1.000000000000000000 ) ) ;
#6738 = CIRCLE ( 'NONE', #3070, 0.1255000000000000282 ) ;
#6739 = CONTEXT_DEPENDENT_SHAPE_REPRESENTATION ( #386, #4154 ) ;
#6740 = VERTEX_POINT ( 'NONE', #6223 ) ;
#6741 = ORIENTED_EDGE ( 'NONE', *, *, #4091, .T. ) ;
#6742 = AXIS2_PLACEMENT_3D ( 'NONE', #6986, #5066, #2675 ) ;
#6743 = ADVANCED_FACE ( 'NONE', ( #3103 ), #6705, .F. ) ;
#6744 = ORIENTED_EDGE ( 'NONE', *, *, #3492, .F. ) ;
#6745 = DIRECTION ( 'NONE',  ( -0.000000000000000000, -0.000000000000000000, -1.000000000000000000 ) ) ;
#6746 = FACE_OUTER_BOUND ( 'NONE', #608, .T. ) ;
#6747 = ADVANCED_FACE ( 'NONE', ( #7322 ), #1052, .T. ) ;
#6748 = CARTESIAN_POINT ( 'NONE',  ( 0.9207653111462810180, 0.7459592875503607834, 0.2179999999999999993 ) ) ;
#6749 = DATE_AND_TIME ( #1862, #6972 ) ;
#6750 = CARTESIAN_POINT ( 'NONE',  ( 0.07000000000000002054, -0.03125000000000000000, 0.8125000000000000000 ) ) ;
#6751 = DIRECTION ( 'NONE',  ( 0.7879377495398141029, 0.6157549048526802515, -0.000000000000000000 ) ) ;
#6752 = AXIS2_PLACEMENT_3D ( 'NONE', #4379, #1254, #3769 ) ;
#6753 = CARTESIAN_POINT ( 'NONE',  ( 1.545700644469172547, 1.253231281308296863, 0.2367370325070441150 ) ) ;
#6754 = CARTESIAN_POINT ( 'NONE',  ( -1.855136387357835481, 0.9645206712600612464, -0.08100000000000007194 ) ) ;
#6755 = APPROVAL ( #5773, 'UNSPECIFIED' ) ;
#6756 = EDGE_CURVE ( 'NONE', #6459, #19, #6053, .T. ) ;
#6757 = AXIS2_PLACEMENT_3D ( 'NONE', #1036, #4037, #5304 ) ;
#6758 = CARTESIAN_POINT ( 'NONE',  ( 6.185915932928153005, 0.4597367884986193753, -0.1250000000000000278 ) ) ;
#6759 = CARTESIAN_POINT ( 'NONE',  ( 0.000000000000000000, 1.425000000000000044, 0.1100000000000000006 ) ) ;
#6760 = DIRECTION ( 'NONE',  ( 0.000000000000000000, 0.000000000000000000, -1.000000000000000000 ) ) ;
#6761 = AXIS2_PLACEMENT_3D ( 'NONE', #3974, #3441, #3481 ) ;
#6762 = ORIENTED_EDGE ( 'NONE', *, *, #7735, .F. ) ;
#6763 = CARTESIAN_POINT ( 'NONE',  ( 1.754394837573727051, 1.324599572866255848, 0.1638240367497202088 ) ) ;
#6764 = VECTOR ( 'NONE', #6528, 39.37007874015748854 ) ;
#6765 = AXIS2_PLACEMENT_3D ( 'NONE', #4933, #6166, #538 ) ;
#6766 = DIRECTION ( 'NONE',  ( -1.000000000000000000, 0.000000000000000000, 0.000000000000000000 ) ) ;
#6767 = PLANE ( 'NONE',  #5466 ) ;
#6768 = APPROVAL_STATUS ( 'not_yet_approved' ) ;
#6769 = ORIENTED_EDGE ( 'NONE', *, *, #719, .F. ) ;
#6770 = DIRECTION ( 'NONE',  ( 0.000000000000000000, 0.000000000000000000, 1.000000000000000000 ) ) ;
#6771 = AXIS2_PLACEMENT_3D ( 'NONE', #3265, #1298, #3807 ) ;
#6772 = ORIENTED_EDGE ( 'NONE', *, *, #6988, .F. ) ;
#6773 = CARTESIAN_POINT ( 'NONE',  ( 3.221700243049673507, 0.8684880333666036289, 5.393636709996481038 ) ) ;
#6774 = TOROIDAL_SURFACE ( 'NONE', #4813, 4.032000000000000917, 0.03200000000000000067 ) ;
#6775 = ORIENTED_EDGE ( 'NONE', *, *, #7844, .F. ) ;
#6776 = VECTOR ( 'NONE', #5758, 39.37007874015748143 ) ;
#6777 = DIRECTION ( 'NONE',  ( -0.7879377495419734867, -0.6157549048499167954, 0.000000000000000000 ) ) ;
#6778 = DIRECTION ( 'NONE',  ( -0.7498009116086186143, 0.6531728565937872100, 0.1056589435873571958 ) ) ;
#6779 = DIRECTION ( 'NONE',  ( -1.000000000000000000, 0.000000000000000000, 0.000000000000000000 ) ) ;
#6780 = ORIENTED_EDGE ( 'NONE', *, *, #1690, .T. ) ;
#6781 = ORIENTED_EDGE ( 'NONE', *, *, #7102, .T. ) ;
#6782 = PERSON ( 'NAUO-PER6', 'UNSPECIFIED', 'UNSPECIFIED', ('UNSPECIFIED'), ('UNSPECIFIED'), ('UNSPECIFIED') ) ;
#6783 = CARTESIAN_POINT ( 'NONE',  ( 0.000000000000000000, 0.6350000000000000089, 0.000000000000000000 ) ) ;
#6784 = LINE ( 'NONE', #4826, #6522 ) ;
#6785 = DIRECTION ( 'NONE',  ( -0.6157549048526801405, 0.7879377495398142139, 0.000000000000000000 ) ) ;
#6786 = PERSON_AND_ORGANIZATION ( #4735, #6190 ) ;
#6787 = LINE ( 'NONE', #7921, #7931 ) ;
#6788 = LINE ( 'NONE', #2353, #7004 ) ;
#6789 = ORIENTED_EDGE ( 'NONE', *, *, #280, .F. ) ;
#6790 = DIRECTION ( 'NONE',  ( -0.000000000000000000, 0.000000000000000000, 1.000000000000000000 ) ) ;
#6791 = DIRECTION ( 'NONE',  ( 0.7879377495398141029, 0.6157549048526801405, 0.000000000000000000 ) ) ;
#6792 = ADVANCED_FACE ( 'NONE', ( #4526 ), #3295, .T. ) ;
#6793 = EDGE_CURVE ( 'NONE', #2684, #7484, #7028, .T. ) ;
#6794 = EDGE_CURVE ( 'NONE', #880, #141, #7520, .T. ) ;
#6795 = DIRECTION ( 'NONE',  ( 0.000000000000000000, 1.000000000000000000, 0.000000000000000000 ) ) ;
#6796 = CARTESIAN_POINT ( 'NONE',  ( 1.315721141621744694, 1.089538881479228838, -0.1203794417438410480 ) ) ;
#6797 = ADVANCED_FACE ( 'NONE', ( #4980 ), #6413, .F. ) ;
#6798 = CARTESIAN_POINT ( 'NONE',  ( 6.067386035484801710, 0.2407470087491039856, -0.1250000000000000000 ) ) ;
#6799 = ORIENTED_EDGE ( 'NONE', *, *, #4182, .T. ) ;
#6800 = ORIENTED_EDGE ( 'NONE', *, *, #2982, .F. ) ;
#6801 = PLANE ( 'NONE',  #2136 ) ;
#6802 = DIRECTION ( 'NONE',  ( 0.7540216022612858948, -0.6568496200222110337, 0.000000000000000000 ) ) ;
#6803 = DIRECTION ( 'NONE',  ( -0.2873478855663425535, -0.000000000000000000, -0.9578262852211522071 ) ) ;
#6804 = DATE_AND_TIME ( #1152, #1450 ) ;
#6805 = EDGE_LOOP ( 'NONE', ( #1285, #7219, #1797, #3634 ) ) ;
#6806 = PLANE ( 'NONE',  #5597 ) ;
#6807 = EDGE_CURVE ( 'NONE', #796, #6698, #6377, .T. ) ;
#6808 = CARTESIAN_POINT ( 'NONE',  ( 3.566133519791359507, 0.3212125039962131501, 0.1850000000000003586 ) ) ;
#6809 = ORIENTED_EDGE ( 'NONE', *, *, #2574, .F. ) ;
#6810 = DIRECTION ( 'NONE',  ( 0.000000000000000000, -0.000000000000000000, 1.000000000000000000 ) ) ;
#6811 = VERTEX_POINT ( 'NONE', #1863 ) ;
#6812 = EDGE_LOOP ( 'NONE', ( #3369, #2014, #5877, #3577, #1768 ) ) ;
#6813 = CARTESIAN_POINT ( 'NONE',  ( 6.067840808230170246, 0.2405569712445295161, -0.1849999999999999978 ) ) ;
#6814 = DIRECTION ( 'NONE',  ( 0.000000000000000000, 0.000000000000000000, -1.000000000000000000 ) ) ;
#6815 = CALENDAR_DATE ( 2026, 9, 10 ) ;
#6816 = SPHERICAL_SURFACE ( 'NONE', #3214, 0.01652128394798136474 ) ;
#6817 = ORIENTED_EDGE ( 'NONE', *, *, #4833, .T. ) ;
#6818 = DIRECTION ( 'NONE',  ( 0.000000000000000000, 0.000000000000000000, -1.000000000000000000 ) ) ;
#6819 = DIRECTION ( 'NONE',  ( -0.7540216022612862279, 0.6568496200222107007, 0.000000000000000000 ) ) ;
#6820 = DIRECTION ( 'NONE',  ( 1.000000000000000000, 0.000000000000000000, -0.000000000000000000 ) ) ;
#6821 = PERSON_AND_ORGANIZATION ( #4735, #6190 ) ;
#6822 = DIRECTION ( 'NONE',  ( 0.7540216022612862279, -0.6568496200222107007, 0.000000000000000000 ) ) ;
#6823 = CARTESIAN_POINT ( 'NONE',  ( 1.878103104100547593, 1.414113082497153728, -0.03271153132810599579 ) ) ;
#6824 = EDGE_LOOP ( 'NONE', ( #6515, #6294, #7888, #3517, #6582 ) ) ;
#6825 = CARTESIAN_POINT ( 'NONE',  ( 0.000000000000000000, 0.6350000000000000089, 0.000000000000000000 ) ) ;
#6826 = DIRECTION ( 'NONE',  ( 1.000000000000000000, 0.000000000000000000, 0.000000000000000000 ) ) ;
#6827 = CARTESIAN_POINT ( 'NONE',  ( 6.067840808230170246, 0.2405569712445295161, -0.1849999999999999978 ) ) ;
#6828 = ADVANCED_FACE ( 'NONE', ( #4486 ), #3219, .T. ) ;
#6829 = EDGE_CURVE ( 'NONE', #1614, #2946, #17, .T. ) ;
#6830 = EDGE_CURVE ( 'NONE', #140, #2070, #1015, .T. ) ;
#6831 = CC_DESIGN_APPROVAL ( #3436, ( #5402 ) ) ;
#6832 = CARTESIAN_POINT ( 'NONE',  ( 0.000000000000000000, 1.050000000000000044, -0.1799999999999999933 ) ) ;
#6833 = ORIENTED_EDGE ( 'NONE', *, *, #7002, .T. ) ;
#6834 = ORIENTED_EDGE ( 'NONE', *, *, #573, .F. ) ;
#6835 = CARTESIAN_POINT ( 'NONE',  ( 1.543631815526617546, 1.159893205310092101, 0.1758941433781722741 ) ) ;
#6836 = VECTOR ( 'NONE', #235, 39.37007874015748143 ) ;
#6837 = CC_DESIGN_DATE_AND_TIME_ASSIGNMENT ( #4308, #6120, ( #172 ) ) ;
#6838 = LOCAL_TIME ( 14, 45, 32.00000000000000000, #4472 ) ;
#6839 = LOCAL_TIME ( 14, 45, 32.00000000000000000, #8000 ) ;
#6840 = EDGE_CURVE ( 'NONE', #761, #2895, #1293, .T. ) ;
#6841 = DIRECTION ( 'NONE',  ( 0.000000000000000000, 0.000000000000000000, -1.000000000000000000 ) ) ;
#6842 = FACE_OUTER_BOUND ( 'NONE', #3252, .T. ) ;
#6843 = DATE_TIME_ROLE ( 'creation_date' ) ;
#6844 = VERTEX_POINT ( 'NONE', #103 ) ;
#6845 = EDGE_CURVE ( 'NONE', #7112, #774, #5135, .T. ) ;
#6846 = VECTOR ( 'NONE', #366, 39.37007874015748143 ) ;
#6847 = DIRECTION ( 'NONE',  ( 0.7983857925064566929, 0.6021462665531003289, -0.000000000000000000 ) ) ;
#6848 = CARTESIAN_POINT ( 'NONE',  ( 6.190221022838899856, 0.4584861219976859026, 5.393636709996481038 ) ) ;
#6849 = CARTESIAN_POINT ( 'NONE',  ( 1.655521228349887242, 1.357097542742190743, 0.2318412895085913417 ) ) ;
#6850 = CIRCLE ( 'NONE', #7886, 0.1875000000000000278 ) ;
#6851 = ORIENTED_EDGE ( 'NONE', *, *, #6794, .T. ) ;
#6852 = LINE ( 'NONE', #4890, #210 ) ;
#6853 = CARTESIAN_POINT ( 'NONE',  ( 1.859753234433174418, 1.471617347716406288, -0.009971652696953780398 ) ) ;
#6854 = CALENDAR_DATE ( 2026, 9, 10 ) ;
#6855 = VECTOR ( 'NONE', #2772, 39.37007874015748854 ) ;
#6856 = VERTEX_POINT ( 'NONE', #6914 ) ;
#6857 = AXIS2_PLACEMENT_3D ( 'NONE', #7645, #7039, #1415 ) ;
#6858 = AXIS2_PLACEMENT_3D ( 'NONE', #183, #62, #7037 ) ;
#6859 = VERTEX_POINT ( 'NONE', #5681 ) ;
#6860 = DIRECTION ( 'NONE',  ( -1.000000000000000000, 0.000000000000000000, 0.000000000000000000 ) ) ;
#6861 = DIRECTION ( 'NONE',  ( -1.000000000000000000, 0.000000000000000000, 0.000000000000000000 ) ) ;
#6862 = UNCERTAINTY_MEASURE_WITH_UNIT (LENGTH_MEASURE( 1.000000000000000082E-05 ), #7989, 'distance_accuracy_value', 'NONE');
#6863 = DIRECTION ( 'NONE',  ( 0.000000000000000000, -0.000000000000000000, -1.000000000000000000 ) ) ;
#6864 = CALENDAR_DATE ( 2026, 9, 10 ) ;
#6865 = DIRECTION ( 'NONE',  ( 0.7879377495398141029, 0.6157549048526802515, 0.000000000000000000 ) ) ;
#6866 = CARTESIAN_POINT ( 'NONE',  ( -0.1250000000000000000, 0.6250000000000000000, 0.03125000000000000000 ) ) ;
#6867 = ORIENTED_EDGE ( 'NONE', *, *, #6552, .T. ) ;
#6868 = CARTESIAN_POINT ( 'NONE',  ( -0.04782642554762442377, -0.07812500000000000000, 0.000000000000000000 ) ) ;
#6869 = CC_DESIGN_SECURITY_CLASSIFICATION ( #187, ( #8100 ) ) ;
#6870 = AXIS2_PLACEMENT_3D ( 'NONE', #4701, #974, #1049 ) ;
#6871 = CIRCLE ( 'NONE', #1504, 0.2923589946935200579 ) ;
#6872 = AXIS2_PLACEMENT_3D ( 'NONE', #983, #7246, #4133 ) ;
#6873 = ORIENTED_EDGE ( 'NONE', *, *, #90, .F. ) ;
#6874 = DIRECTION ( 'NONE',  ( -1.000000000000000000, 0.000000000000000000, 0.000000000000000000 ) ) ;
#6875 = CARTESIAN_POINT ( 'NONE',  ( 1.348222454147280480, 1.073204572620011898, -0.1377597263139525574 ) ) ;
#6876 = DIRECTION ( 'NONE',  ( 0.000000000000000000, 0.000000000000000000, -1.000000000000000000 ) ) ;
#6877 = VERTEX_POINT ( 'NONE', #57 ) ;
#6878 = CARTESIAN_POINT ( 'NONE',  ( -0.03125000000000000000, 0.03125000000000000000, -0.1204106507132265275 ) ) ;
#6879 = CIRCLE ( 'NONE', #5969, 0.3024878104020024550 ) ;
#6880 = ORIENTED_EDGE ( 'NONE', *, *, #7687, .T. ) ;
#6881 = ADVANCED_FACE ( 'NONE', ( #2594 ), #3766, .T. ) ;
#6882 = ORIENTED_EDGE ( 'NONE', *, *, #5244, .T. ) ;
#6883 = DIRECTION ( 'NONE',  ( -0.000000000000000000, 1.000000000000000000, -0.000000000000000000 ) ) ;
#6884 = PLANE ( 'NONE',  #6269 ) ;
#6885 = AXIS2_PLACEMENT_3D ( 'NONE', #5745, #660, #3 ) ;
#6886 = APPROVAL_ROLE ( '' ) ;
#6887 = ORIENTED_EDGE ( 'NONE', *, *, #1577, .F. ) ;
#6888 = CARTESIAN_POINT ( 'NONE',  ( 1.388198106678872445, 1.072068126535121069, -0.1818941674207988357 ) ) ;
#6889 = CARTESIAN_POINT ( 'NONE',  ( -0.6148017326439689789, 0.2092266780087954636, 0.2500000000000000000 ) ) ;
#6890 = EDGE_LOOP ( 'NONE', ( #972, #4613, #2430, #6014 ) ) ;
#6891 = VECTOR ( 'NONE', #4709, 39.37007874015748143 ) ;
#6892 = CARTESIAN_POINT ( 'NONE',  ( 0.000000000000000000, 0.5625000000000000000, 0.000000000000000000 ) ) ;
#6893 = AXIS2_PLACEMENT_3D ( 'NONE', #1850, #7988, #6898 ) ;
#6894 = ADVANCED_FACE ( 'NONE', ( #3257 ), #6774, .T. ) ;
#6895 = ORIENTED_EDGE ( 'NONE', *, *, #5052, .F. ) ;
#6896 = ORIENTED_EDGE ( 'NONE', *, *, #5787, .T. ) ;
#6897 = ORIENTED_EDGE ( 'NONE', *, *, #573, .T. ) ;
#6898 = DIRECTION ( 'NONE',  ( 1.000000000000000000, 0.000000000000000000, 0.000000000000000000 ) ) ;
#6899 = DIRECTION ( 'NONE',  ( -0.6568496200222101455, -0.7540216022612868940, -1.582067810090848465E-15 ) ) ;
#6900 = CYLINDRICAL_SURFACE ( 'NONE', #4637, 0.06250000000000000000 ) ;
#6901 = CC_DESIGN_PERSON_AND_ORGANIZATION_ASSIGNMENT ( #3896, #1928, ( #6511 ) ) ;
#6902 = FACE_OUTER_BOUND ( 'NONE', #610, .T. ) ;
#6903 = EDGE_CURVE ( 'NONE', #7381, #4068, #5464, .T. ) ;
#6904 = EDGE_LOOP ( 'NONE', ( #1332, #6234, #4999, #5509, #1933, #1082, #5352, #7707, #7430 ) ) ;
#6905 = VECTOR ( 'NONE', #6679, 39.37007874015748143 ) ;
#6906 = ORIENTED_EDGE ( 'NONE', *, *, #4203, .F. ) ;
#6907 = AXIS2_PLACEMENT_3D ( 'NONE', #1562, #4806, #332 ) ;
#6908 = VERTEX_POINT ( 'NONE', #2022 ) ;
#6909 = CARTESIAN_POINT ( 'NONE',  ( 0.000000000000000000, 0.6350000000000000089, -0.1150000000000000050 ) ) ;
#6910 = CARTESIAN_POINT ( 'NONE',  ( -0.1054677083281892608, 0.5625000000000000000, -0.03125000000000000000 ) ) ;
#6912 = DIRECTION ( 'NONE',  ( -0.6157549048526804736, 0.7879377495398138809, 0.000000000000000000 ) ) ;
#6911 = AXIS2_PLACEMENT_3D ( 'NONE', #7580, #7009, #119 ) ;
#6913 = PERSON_AND_ORGANIZATION ( #4735, #6190 ) ;
#6914 = CARTESIAN_POINT ( 'NONE',  ( 1.258671604940864608, -0.02501003737716508274, -0.1849999999999999978 ) ) ;
#6915 = CARTESIAN_POINT ( 'NONE',  ( -6.110602001756019419, -1.404684638105634820, 0.3125000000000000000 ) ) ;
#6916 = ORIENTED_EDGE ( 'NONE', *, *, #7844, .T. ) ;
#6917 = VERTEX_POINT ( 'NONE', #5760 ) ;
#6918 = ORIENTED_EDGE ( 'NONE', *, *, #4786, .T. ) ;
#6919 = CARTESIAN_POINT ( 'NONE',  ( -0.03125000000000000000, 0.000000000000000000, -0.1106726592253027830 ) ) ;
#6920 = DIRECTION ( 'NONE',  ( 0.8680936205257663296, -0.4964005096718443477, 0.000000000000000000 ) ) ;
#6921 = EDGE_CURVE ( 'NONE', #1342, #2815, #2055, .T. ) ;
#6922 = CARTESIAN_POINT ( 'NONE',  ( -1.420319797626316216, 0.8334728170008732784, 0.1249999999999995559 ) ) ;
#6923 = DIRECTION ( 'NONE',  ( -0.000000000000000000, -1.000000000000000000, -0.000000000000000000 ) ) ;
#6924 = ORIENTED_EDGE ( 'NONE', *, *, #3395, .T. ) ;
#6925 = DIRECTION ( 'NONE',  ( -1.000000000000000000, 0.000000000000000000, 0.000000000000000000 ) ) ;
#6926 = DIRECTION ( 'NONE',  ( 0.000000000000000000, 1.000000000000000000, 0.000000000000000000 ) ) ;
#6927 = COORDINATED_UNIVERSAL_TIME_OFFSET ( 0, 0, .AHEAD. ) ;
#6928 = ORIENTED_EDGE ( 'NONE', *, *, #634, .F. ) ;
#6929 = DIRECTION ( 'NONE',  ( 0.000000000000000000, -0.000000000000000000, -1.000000000000000000 ) ) ;
#6930 = DIRECTION ( 'NONE',  ( -1.000000000000000000, 0.000000000000000000, 0.000000000000000000 ) ) ;
#6931 = EDGE_CURVE ( 'NONE', #5067, #6939, #788, .T. ) ;
#6932 = CARTESIAN_POINT ( 'NONE',  ( 1.466665248995881354, 0.6909135088951505743, 0.1250000000000000000 ) ) ;
#6933 = CARTESIAN_POINT ( 'NONE',  ( -4.882388066182516084, 5.670153330992327767, 0.3125000000000000000 ) ) ;
#6934 = MECHANICAL_CONTEXT ( 'NONE', #4314, 'mechanical' ) ;
#6935 = CARTESIAN_POINT ( 'NONE',  ( -0.09374999999999998612, 1.148106374200643401E-17, 0.1250000000000000000 ) ) ;
#6936 = EDGE_CURVE ( 'NONE', #2236, #4588, #2852, .T. ) ;
#6937 = DIRECTION ( 'NONE',  ( -0.000000000000000000, -1.000000000000000000, -0.000000000000000000 ) ) ;
#6938 = ADVANCED_FACE ( 'NONE', ( #4567 ), #5883, .F. ) ;
#6939 = VERTEX_POINT ( 'NONE', #7307 ) ;
#6940 = CC_DESIGN_DATE_AND_TIME_ASSIGNMENT ( #631, #3667, ( #51 ) ) ;
#6941 = ORIENTED_EDGE ( 'NONE', *, *, #4684, .F. ) ;
#6942 = EDGE_CURVE ( 'NONE', #3224, #2946, #1147, .T. ) ;
#6943 = VERTEX_POINT ( 'NONE', #260 ) ;
#6944 = ORIENTED_EDGE ( 'NONE', *, *, #522, .F. ) ;
#6945 = EDGE_CURVE ( 'NONE', #1252, #6574, #3500, .T. ) ;
#6946 =( NAMED_UNIT ( * ) SI_UNIT ( $, .STERADIAN. ) SOLID_ANGLE_UNIT ( ) );
#6947 = DIRECTION ( 'NONE',  ( -0.000000000000000000, -0.000000000000000000, 1.000000000000000000 ) ) ;
#6948 = APPROVAL_DATE_TIME ( #1443, #5548 ) ;
#6949 = DIRECTION ( 'NONE',  ( 1.000000000000000000, 0.000000000000000000, 0.000000000000000000 ) ) ;
#6950 = DIRECTION ( 'NONE',  ( -0.000000000000000000, -0.000000000000000000, 1.000000000000000000 ) ) ;
#6951 = EDGE_LOOP ( 'NONE', ( #6327, #266, #446, #2933 ) ) ;
#6952 = EDGE_CURVE ( 'NONE', #1018, #6628, #7685, .T. ) ;
#6953 = FACE_OUTER_BOUND ( 'NONE', #6537, .T. ) ;
#6954 = ORIENTED_EDGE ( 'NONE', *, *, #6830, .T. ) ;
#6955 = CARTESIAN_POINT ( 'NONE',  ( 1.556400554713971651, 1.293514327272109687, 0.2500000000000000000 ) ) ;
#6956 = DIRECTION ( 'NONE',  ( -0.000000000000000000, -0.000000000000000000, -1.000000000000000000 ) ) ;
#6957 = FACE_OUTER_BOUND ( 'NONE', #3471, .T. ) ;
#6958 = CARTESIAN_POINT ( 'NONE',  ( -1.484384414703910027, 0.9067922411947360040, 0.1720737575213688586 ) ) ;
#6959 = SECURITY_CLASSIFICATION ( '', '', #2219 ) ;
#6960 = VECTOR ( 'NONE', #2065, 39.37007874015748143 ) ;
#6961 = CYLINDRICAL_SURFACE ( 'NONE', #2413, 0.2149999999999995803 ) ;
#6962 = APPROVAL_PERSON_ORGANIZATION ( #282, #2739, #2088 ) ;
#6963 = DIRECTION ( 'NONE',  ( 0.6568496200222107007, 0.7540216022612862279, -0.000000000000000000 ) ) ;
#6964 = DATE_AND_TIME ( #3815, #2903 ) ;
#6965 = ORIENTED_EDGE ( 'NONE', *, *, #7796, .F. ) ;
#6966 = CARTESIAN_POINT ( 'NONE',  ( 0.000000000000000000, 0.000000000000000000, 0.09374999999999998612 ) ) ;
#6967 = DIRECTION ( 'NONE',  ( -0.6157549048526823610, 0.7879377495398123266, 0.000000000000000000 ) ) ;
#6968 = VECTOR ( 'NONE', #6876, 39.37007874015748143 ) ;
#6969 = ORIENTED_EDGE ( 'NONE', *, *, #1936, .T. ) ;
#6970 = CARTESIAN_POINT ( 'NONE',  ( 5.983714301115757195, -0.05774751952986827835, 0.1850000000000003586 ) ) ;
#6971 = AXIS2_PLACEMENT_3D ( 'NONE', #4040, #6615, #5313 ) ;
#6972 = LOCAL_TIME ( 14, 45, 32.00000000000000000, #1825 ) ;
#6973 = CIRCLE ( 'NONE', #1613, 0.03124999999999997571 ) ;
#6974 = DIRECTION ( 'NONE',  ( -1.000000000000000000, -6.975840231036812635E-15, 0.000000000000000000 ) ) ;
#6975 = CARTESIAN_POINT ( 'NONE',  ( -4.882388066182494768, 5.670153330992220297, 0.3125000000000000000 ) ) ;
#6976 = DIRECTION ( 'NONE',  ( 0.000000000000000000, 1.000000000000000000, 0.000000000000000000 ) ) ;
#6977 = VECTOR ( 'NONE', #1104, 39.37007874015748143 ) ;
#6978 = EDGE_LOOP ( 'NONE', ( #6145, #7295, #5836, #2267 ) ) ;
#6979 = EDGE_CURVE ( 'NONE', #6311, #7663, #836, .T. ) ;
#6980 = EDGE_LOOP ( 'NONE', ( #1262, #1617, #6396, #3226 ) ) ;
#6981 = DIRECTION ( 'NONE',  ( 0.000000000000000000, 0.000000000000000000, 1.000000000000000000 ) ) ;
#6982 = VECTOR ( 'NONE', #415, 39.37007874015748143 ) ;
#6983 = DIRECTION ( 'NONE',  ( 0.000000000000000000, 0.000000000000000000, -1.000000000000000000 ) ) ;
#6984 = ITEM_DEFINED_TRANSFORMATION ( 'NONE', 'NONE', #2642,  #3555 ) ;
#6985 = CARTESIAN_POINT ( 'NONE',  ( 6.067385397437120353, 0.2407432673787524013, -0.1849999999999999978 ) ) ;
#6986 = CARTESIAN_POINT ( 'NONE',  ( 0.000000000000000000, 0.03124999999999997571, 0.000000000000000000 ) ) ;
#6987 = ORIENTED_EDGE ( 'NONE', *, *, #6794, .F. ) ;
#6988 = EDGE_CURVE ( 'NONE', #7717, #3019, #98, .T. ) ;
#6989 = VECTOR ( 'NONE', #937, 39.37007874015748143 ) ;
#6990 = CIRCLE ( 'NONE', #6858, 0.03200000000000011169 ) ;
#6991 = ADVANCED_FACE ( 'NONE', ( #4847 ), #7260, .F. ) ;
#6992 = ORIENTED_EDGE ( 'NONE', *, *, #4340, .F. ) ;
#6993 = DIRECTION ( 'NONE',  ( -0.000000000000000000, -1.000000000000000000, -0.000000000000000000 ) ) ;
#6994 = ORIENTED_EDGE ( 'NONE', *, *, #126, .T. ) ;
#6995 = EDGE_CURVE ( 'NONE', #445, #3298, #4677, .T. ) ;
#6996 = CARTESIAN_POINT ( 'NONE',  ( 1.472947776714219836, 0.7825821671288679671, -0.1849999999999999978 ) ) ;
#6997 = DIRECTION ( 'NONE',  ( 0.000000000000000000, 0.000000000000000000, -1.000000000000000000 ) ) ;
#6998 = LOCAL_TIME ( 14, 45, 32.00000000000000000, #5592 ) ;
#6999 = AXIS2_PLACEMENT_3D ( 'NONE', #4416, #5219, #7745 ) ;
#7000 = CC_DESIGN_DATE_AND_TIME_ASSIGNMENT ( #2021, #2067, ( #1471 ) ) ;
#7001 = CARTESIAN_POINT ( 'NONE',  ( 1.821876573136023136, 1.470292042915513520, 0.07759758242713811482 ) ) ;
#7002 = EDGE_CURVE ( 'NONE', #713, #6811, #4605, .T. ) ;
#7003 = CARTESIAN_POINT ( 'NONE',  ( 3.672798492683009286, -8.252032378159654513, 5.393636709996481038 ) ) ;
#7004 = VECTOR ( 'NONE', #643, 39.37007874015748143 ) ;
#7005 = CARTESIAN_POINT ( 'NONE',  ( 1.779809833619593773, 1.437619977954180950, 0.1424345704801376344 ) ) ;
#7006 = PLANE ( 'NONE',  #2565 ) ;
#7007 = DATE_TIME_ROLE ( 'creation_date' ) ;
#7008 = ORIENTED_EDGE ( 'NONE', *, *, #2374, .T. ) ;
#7009 = DIRECTION ( 'NONE',  ( -0.000000000000000000, -1.000000000000000000, -0.000000000000000000 ) ) ;
#7010 = CARTESIAN_POINT ( 'NONE',  ( -1.222146065255383940, -0.1443597716867830172, -0.05999999999999999778 ) ) ;
#7011 = CIRCLE ( 'NONE', #4131, 0.03125000000000000694 ) ;
#7012 = ORIENTED_EDGE ( 'NONE', *, *, #2936, .F. ) ;
#7013 = ORIENTED_EDGE ( 'NONE', *, *, #2134, .T. ) ;
#7014 = PLANE ( 'NONE',  #5137 ) ;
#7015 = DIRECTION ( 'NONE',  ( 0.000000000000000000, 0.000000000000000000, -1.000000000000000000 ) ) ;
#7016 = APPROVAL_DATE_TIME ( #4515, #3436 ) ;
#7017 = DIRECTION ( 'NONE',  ( -0.000000000000000000, 0.000000000000000000, -1.000000000000000000 ) ) ;
#7018 = AXIS2_PLACEMENT_3D ( 'NONE', #7487, #487, #6716 ) ;
#7019 = CARTESIAN_POINT ( 'NONE',  ( 1.535166674676289089, 1.856143143388933492, -5.593666872230160467E-06 ) ) ;
#7020 = CARTESIAN_POINT ( 'NONE',  ( 1.715112207380193654, 1.389698554653518103, 0.2327866256051912830 ) ) ;
#7021 = TOROIDAL_SURFACE ( 'NONE', #3098, 0.1523203157102362704, 0.06250000000000000000 ) ;
#7022 = VECTOR ( 'NONE', #6521, 39.37007874015748143 ) ;
#7023 = CIRCLE ( 'NONE', #4152, 0.09374999999999998612 ) ;
#7024 = ORIENTED_EDGE ( 'NONE', *, *, #2134, .F. ) ;
#7025 = DIRECTION ( 'NONE',  ( 0.000000000000000000, 0.000000000000000000, -1.000000000000000000 ) ) ;
#7026 = CARTESIAN_POINT ( 'NONE',  ( 0.1250000000000000278, 0.03125000000000000000, 0.06250000000000000000 ) ) ;
#7027 = DATE_AND_TIME ( #3256, #1991 ) ;
#7028 = LINE ( 'NONE', #3913, #6639 ) ;
#7029 = DIRECTION ( 'NONE',  ( -0.000000000000000000, -0.000000000000000000, -1.000000000000000000 ) ) ;
#7030 = ORIENTED_EDGE ( 'NONE', *, *, #4142, .F. ) ;
#7031 = AXIS2_PLACEMENT_3D ( 'NONE', #2105, #1686, #3389 ) ;
#7032 = ORIENTED_EDGE ( 'NONE', *, *, #5739, .T. ) ;
#7033 = ORIENTED_EDGE ( 'NONE', *, *, #882, .T. ) ;
#7034 = AXIS2_PLACEMENT_3D ( 'NONE', #6966, #5254, #2090 ) ;
#7035 = ORIENTED_EDGE ( 'NONE', *, *, #1536, .F. ) ;
#7036 = AXIS2_PLACEMENT_3D ( 'NONE', #7138, #1032, #1520 ) ;
#7037 = DIRECTION ( 'NONE',  ( -0.5035814659566155704, 0.8639477456102226949, 0.000000000000000000 ) ) ;
#7038 = ORIENTED_EDGE ( 'NONE', *, *, #3187, .T. ) ;
#7039 = DIRECTION ( 'NONE',  ( 0.6568496200222107007, 0.7540216022612863389, -0.000000000000000000 ) ) ;
#7040 = DIRECTION ( 'NONE',  ( 0.000000000000000000, 0.000000000000000000, 1.000000000000000000 ) ) ;
#7041 = EDGE_CURVE ( 'NONE', #3041, #5878, #3342, .T. ) ;
#7042 = CARTESIAN_POINT ( 'NONE',  ( -1.275477614966805673, 0.03477957369036089458, 0.2500000000000000000 ) ) ;
#7043 = EDGE_CURVE ( 'NONE', #3946, #1218, #1641, .T. ) ;
#7044 = ORIENTED_EDGE ( 'NONE', *, *, #781, .F. ) ;
#7045 = FACE_OUTER_BOUND ( 'NONE', #1986, .T. ) ;
#7046 = ORIENTED_EDGE ( 'NONE', *, *, #1835, .F. ) ;
#7047 = EDGE_CURVE ( 'NONE', #5362, #6459, #1399, .T. ) ;
#7048 = CARTESIAN_POINT ( 'NONE',  ( 6.067840808230170246, 0.2405569712445295161, -0.1250000000000004441 ) ) ;
#7049 = CARTESIAN_POINT ( 'NONE',  ( 1.590963538254601684, 1.298412701918328915, -0.1039999999999998703 ) ) ;
#7050 = DATE_TIME_ROLE ( 'classification_date' ) ;
#7051 = ORIENTED_EDGE ( 'NONE', *, *, #528, .T. ) ;
#7052 = DIRECTION ( 'NONE',  ( 0.9968059542140783602, 0.000000000000000000, 0.07986169071188227442 ) ) ;
#7053 = LINE ( 'NONE', #7739, #3487 ) ;
#7054 = ORIENTED_EDGE ( 'NONE', *, *, #6298, .T. ) ;
#7055 = CARTESIAN_POINT ( 'NONE',  ( -1.723766588794375387, 1.115324847714046497, -0.08100000000000007194 ) ) ;
#7056 = CARTESIAN_POINT ( 'NONE',  ( 0.2796912674003787513, -4.528516545235624413, 0.03199999999999999373 ) ) ;
#7057 = CARTESIAN_POINT ( 'NONE',  ( 0.1250000000000000278, 0.03125000000000000000, 0.06250000000000000000 ) ) ;
#7058 = CALENDAR_DATE ( 2026, 9, 10 ) ;
#7059 = DIRECTION ( 'NONE',  ( -1.000000000000000000, 0.000000000000000000, 0.000000000000000000 ) ) ;
#7060 = DIRECTION ( 'NONE',  ( -1.000000000000000000, 0.000000000000000000, 0.000000000000000000 ) ) ;
#7061 = CARTESIAN_POINT ( 'NONE',  ( 1.452776126472616669, 1.185506347939969674, 0.2257575757582501175 ) ) ;
#7062 = VERTEX_POINT ( 'NONE', #3617 ) ;
#7063 = VERTEX_POINT ( 'NONE', #7108 ) ;
#7064 = CARTESIAN_POINT ( 'NONE',  ( 0.03125000000000000000, 0.000000000000000000, 0.000000000000000000 ) ) ;
#7065 = PERSON_AND_ORGANIZATION ( #4735, #6190 ) ;
#7066 = CARTESIAN_POINT ( 'NONE',  ( 0.9690125299525020885, 0.8529848947786566882, 0.03200000000000000067 ) ) ;
#7067 = CARTESIAN_POINT ( 'NONE',  ( -0.09999999999999997780, -0.03125000000000000000, 0.7124999999999989120 ) ) ;
#7068 = ORIENTED_EDGE ( 'NONE', *, *, #2528, .F. ) ;
#7069 = ORIENTED_EDGE ( 'NONE', *, *, #1319, .T. ) ;
#7070 = EDGE_LOOP ( 'NONE', ( #2962, #2097, #3749, #5140, #3392, #2762, #5483, #6944 ) ) ;
#7071 = ORIENTED_EDGE ( 'NONE', *, *, #6043, .F. ) ;
#7072 = LINE ( 'NONE', #1413, #4115 ) ;
#7073 = ORIENTED_EDGE ( 'NONE', *, *, #2457, .F. ) ;
#7074 = CARTESIAN_POINT ( 'NONE',  ( 1.637040878673387878, 1.317643376044983938, 0.2304635611191261646 ) ) ;
#7075 = DIRECTION ( 'NONE',  ( 0.000000000000000000, 0.000000000000000000, 1.000000000000000000 ) ) ;
#7076 = LINE ( 'NONE', #2078, #3953 ) ;
#7077 = DIRECTION ( 'NONE',  ( 1.224646799147352961E-16, 0.000000000000000000, -1.000000000000000000 ) ) ;
#7078 = EDGE_CURVE ( 'NONE', #7153, #375, #177, .T. ) ;
#7079 = EDGE_CURVE ( 'NONE', #873, #4304, #5989, .T. ) ;
#7080 = CARTESIAN_POINT ( 'NONE',  ( 1.386772069378664041, 1.773409745440035934, 0.2021634589242503610 ) ) ;
#7081 = FACE_OUTER_BOUND ( 'NONE', #5234, .T. ) ;
#7082 = DATE_AND_TIME ( #3365, #1329 ) ;
#7083 = DIRECTION ( 'NONE',  ( 0.000000000000000000, 0.000000000000000000, 1.000000000000000000 ) ) ;
#7084 = LINE ( 'NONE', #2174, #6510 ) ;
#7085 = EDGE_CURVE ( 'NONE', #5716, #4569, #2068, .T. ) ;
#7086 = CARTESIAN_POINT ( 'NONE',  ( 0.3566525292043905560, -0.3408511508279104540, 0.02836266418265003669 ) ) ;
#7087 = ORIENTED_EDGE ( 'NONE', *, *, #6043, .T. ) ;
#7088 = LINE ( 'NONE', #4031, #6455 ) ;
#7089 = CC_DESIGN_PERSON_AND_ORGANIZATION_ASSIGNMENT ( #2182, #3448, ( #3286 ) ) ;
#7090 = EDGE_CURVE ( 'NONE', #1621, #658, #6503, .T. ) ;
#7091 = EDGE_CURVE ( 'NONE', #4299, #646, #619, .T. ) ;
#7092 = ADVANCED_FACE ( 'NONE', ( #405 ), #6806, .F. ) ;
#7093 = CARTESIAN_POINT ( 'NONE',  ( 1.475891671935536609, 0.7226544316391472211, 0.09375000000000005551 ) ) ;
#7094 = CARTESIAN_POINT ( 'NONE',  ( 1.494844024332783405, 1.818976347620703704, 0.1550510257216821397 ) ) ;
#7095 = APPROVAL_STATUS ( 'not_yet_approved' ) ;
#7096 = EDGE_LOOP ( 'NONE', ( #2878, #3105, #3483, #5719, #5465, #1103, #2108, #551 ) ) ;
#7097 = CARTESIAN_POINT ( 'NONE',  ( 1.490632003353124846, 1.854573852375907217, -0.03652564415615681959 ) ) ;
#7098 = AXIS2_PLACEMENT_3D ( 'NONE', #3785, #3248, #2662 ) ;
#7099 = CARTESIAN_POINT ( 'NONE',  ( 0.2935750530104211387, 0.05119392622207447063, 0.000000000000000000 ) ) ;
#7100 = CC_DESIGN_APPROVAL ( #4341, ( #1857 ) ) ;
#7101 = ADVANCED_FACE ( 'NONE', ( #6200 ), #7424, .T. ) ;
#7102 = EDGE_CURVE ( 'NONE', #1684, #2487, #7981, .T. ) ;
#7103 = AXIS2_PLACEMENT_3D ( 'NONE', #5050, #4511, #6398 ) ;
#7104 = ORIENTED_EDGE ( 'NONE', *, *, #906, .F. ) ;
#7105 = ORIENTED_EDGE ( 'NONE', *, *, #6328, .T. ) ;
#7106 = CARTESIAN_POINT ( 'NONE',  ( 1.475891671935536609, 0.7226544316391472211, 5.393636709996481038 ) ) ;
#7107 = DIRECTION ( 'NONE',  ( 1.000000000000000000, 0.000000000000000000, 0.000000000000000000 ) ) ;
#7108 = CARTESIAN_POINT ( 'NONE',  ( -1.023858060246952029, -0.8104042351526981047, 0.3125000000000000000 ) ) ;
#7109 = CARTESIAN_POINT ( 'NONE',  ( 1.530808498934191201E-17, 0.6124999999999999334, -0.1250000000000000000 ) ) ;
#7110 = AXIS2_PLACEMENT_3D ( 'NONE', #7855, #1592, #6640 ) ;
#7111 = ORIENTED_EDGE ( 'NONE', *, *, #6033, .T. ) ;
#7112 = VERTEX_POINT ( 'NONE', #4437 ) ;
#7113 = EDGE_LOOP ( 'NONE', ( #2916, #7104, #6954, #917 ) ) ;
#7114 = EDGE_LOOP ( 'NONE', ( #5479, #3337 ) ) ;
#7115 = AXIS2_PLACEMENT_3D ( 'NONE', #257, #347, #4160 ) ;
#7116 = ORIENTED_EDGE ( 'NONE', *, *, #7440, .T. ) ;
#7117 = ORIENTED_EDGE ( 'NONE', *, *, #670, .T. ) ;
#7118 = CYLINDRICAL_SURFACE ( 'NONE', #7640, 0.1100000000000000006 ) ;
#7119 = ORIENTED_EDGE ( 'NONE', *, *, #2612, .F. ) ;
#7120 = CARTESIAN_POINT ( 'NONE',  ( 3.221700243049672174, 0.8684880333666047392, 5.393636709996481038 ) ) ;
#7121 = PLANE ( 'NONE',  #4931 ) ;
#7122 = FACE_OUTER_BOUND ( 'NONE', #5280, .T. ) ;
#7123 = TOROIDAL_SURFACE ( 'NONE', #3584, 0.1487499999999999933, 0.03125000000000000000 ) ;
#7124 = ORIENTED_EDGE ( 'NONE', *, *, #438, .F. ) ;
#7125 = CIRCLE ( 'NONE', #3724, 0.03200000000000000067 ) ;
#7126 = CARTESIAN_POINT ( 'NONE',  ( 3.672767464462126430, -8.314346814944791220, -0.1849999999999999978 ) ) ;
#7127 = ORGANIZATION ( 'NAUO-ORG8', 'UNSPECIFIED', 'UNSPECIFIED' ) ;
#7128 = AXIS2_PLACEMENT_3D ( 'NONE', #2204, #6583, #427 ) ;
#7129 = FACE_OUTER_BOUND ( 'NONE', #5601, .T. ) ;
#7130 = DIRECTION ( 'NONE',  ( -0.6157549048542445558, 0.7879377495385916363, 0.000000000000000000 ) ) ;
#7131 = COORDINATED_UNIVERSAL_TIME_OFFSET ( 0, 0, .AHEAD. ) ;
#7132 = DIRECTION ( 'NONE',  ( -0.07966912593697374201, 0.06940203694730361084, 0.9944024274105548455 ) ) ;
#7133 = DIRECTION ( 'NONE',  ( 0.7498009116086189474, -0.6531728565937869879, 0.1056589435873569599 ) ) ;
#7134 = ORIENTED_EDGE ( 'NONE', *, *, #3791, .T. ) ;
#7135 = FACE_OUTER_BOUND ( 'NONE', #5166, .T. ) ;
#7136 = TOROIDAL_SURFACE ( 'NONE', #5564, 0.4024878104020024328, 0.1000000000000000056 ) ;
#7137 = CARTESIAN_POINT ( 'NONE',  ( 1.421781027083512505, 1.064669666792219527, -0.2249973011472257700 ) ) ;
#7138 = CARTESIAN_POINT ( 'NONE',  ( 0.000000000000000000, -0.03125000000000000000, 0.6646281645421511231 ) ) ;
#7139 = VECTOR ( 'NONE', #1612, 39.37007874015748143 ) ;
#7140 = PERSON_AND_ORGANIZATION_ROLE ( 'creator' ) ;
#7141 = VERTEX_POINT ( 'NONE', #533 ) ;
#7142 = AXIS2_PLACEMENT_3D ( 'NONE', #4955, #4332, #686 ) ;
#7143 = VERTEX_POINT ( 'NONE', #3780 ) ;
#7144 = CARTESIAN_POINT ( 'NONE',  ( 2.023273750469992349E-18, 0.03125000000000000000, 0.6811494484901324808 ) ) ;
#7145 = LINE ( 'NONE', #957, #429 ) ;
#7146 = ADVANCED_FACE ( 'NONE', ( #1810 ), #894, .T. ) ;
#7147 = ADVANCED_FACE ( 'NONE', ( #1154, #6161 ), #4883, .T. ) ;
#7148 = CIRCLE ( 'NONE', #3750, 9.004497838701050583 ) ;
#7149 = EDGE_CURVE ( 'NONE', #3663, #5927, #2492, .T. ) ;
#7150 = ORIENTED_EDGE ( 'NONE', *, *, #5895, .T. ) ;
#7151 = EDGE_CURVE ( 'NONE', #1559, #822, #3637, .T. ) ;
#7152 = LENGTH_MEASURE_WITH_UNIT ( LENGTH_MEASURE( 0.02539999999999999897 ), #5355 );
#7153 = VERTEX_POINT ( 'NONE', #2410 ) ;
#7154 = LINE ( 'NONE', #6577, #5150 ) ;
#7155 = DIRECTION ( 'NONE',  ( 0.000000000000000000, 0.000000000000000000, -1.000000000000000000 ) ) ;
#7156 = APPROVAL_DATE_TIME ( #2920, #6203 ) ;
#7157 = LINE ( 'NONE', #6012, #4007 ) ;
#7158 = CIRCLE ( 'NONE', #1129, 0.4999999999999997224 ) ;
#7159 = ORIENTED_EDGE ( 'NONE', *, *, #1941, .F. ) ;
#7160 = TOROIDAL_SURFACE ( 'NONE', #4280, 0.1255000000000000282, 0.06199999999999999956 ) ;
#7161 = ORIENTED_EDGE ( 'NONE', *, *, #5086, .F. ) ;
#7162 = AXIS2_PLACEMENT_3D ( 'NONE', #5711, #93, #5168 ) ;
#7163 = PRODUCT_DEFINITION_SHAPE ( 'NONE', 'NONE',  #8096 ) ;
#7164 = ORIENTED_EDGE ( 'NONE', *, *, #993, .F. ) ;
#7165 = ORIENTED_EDGE ( 'NONE', *, *, #3403, .T. ) ;
#7166 = DIRECTION ( 'NONE',  ( 0.000000000000000000, 0.000000000000000000, 1.000000000000000000 ) ) ;
#7167 = VERTEX_POINT ( 'NONE', #4350 ) ;
#7169 = LINE ( 'NONE', #3515, #6077 ) ;
#7168 = CIRCLE ( 'NONE', #4675, 0.1250000000000001110 ) ;
#7170 = DIRECTION ( 'NONE',  ( 1.000000000000000000, 0.000000000000000000, 0.000000000000000000 ) ) ;
#7171 = CARTESIAN_POINT ( 'NONE',  ( 0.1000000000000000472, -0.03125000000000000000, 0.8125000000000000000 ) ) ;
#7172 = DIRECTION ( 'NONE',  ( 0.000000000000000000, 0.000000000000000000, -1.000000000000000000 ) ) ;
#7173 = VECTOR ( 'NONE', #1191, 39.37007874015748143 ) ;
#7174 = CIRCLE ( 'NONE', #7693, 0.03124999999999997571 ) ;
#7175 = DIRECTION ( 'NONE',  ( 1.000000000000000000, -2.283006407345790279E-13, 0.000000000000000000 ) ) ;
#7176 = FACE_OUTER_BOUND ( 'NONE', #7472, .T. ) ;
#7177 = CARTESIAN_POINT ( 'NONE',  ( 0.2976660692273699338, -0.3850326757561698954, 0.000000000000000000 ) ) ;
#7178 = EDGE_LOOP ( 'NONE', ( #3547, #7839 ) ) ;
#7179 = CARTESIAN_POINT ( 'NONE',  ( -0.1250000000000000000, 0.5625000000000000000, -0.03125000000000000000 ) ) ;
#7180 = ADVANCED_BREP_SHAPE_REPRESENTATION ( '', ( #3575, #3555 ), #6058 ) ;
#7181 = CARTESIAN_POINT ( 'NONE',  ( 1.854131197359395689, 1.310528858172997690, -0.1039999999999998703 ) ) ;
#7182 = CARTESIAN_POINT ( 'NONE',  ( 1.611351012831676144, 0.9234512119983975253, -0.1039999999999998287 ) ) ;
#7183 = COORDINATED_UNIVERSAL_TIME_OFFSET ( 0, 0, .AHEAD. ) ;
#7184 = VERTEX_POINT ( 'NONE', #6284 ) ;
#7185 = DIRECTION ( 'NONE',  ( -1.000000000000000000, 0.000000000000000000, 0.000000000000000000 ) ) ;
#7186 = DIRECTION ( 'NONE',  ( -0.000000000000000000, 0.000000000000000000, 1.000000000000000000 ) ) ;
#7187 = VERTEX_POINT ( 'NONE', #2368 ) ;
#7188 = ORIENTED_EDGE ( 'NONE', *, *, #578, .F. ) ;
#7189 = ADVANCED_FACE ( 'NONE', ( #3659 ), #6243, .T. ) ;
#7190 = DIRECTION ( 'NONE',  ( 0.000000000000000000, 0.000000000000000000, 1.000000000000000000 ) ) ;
#7191 = VERTEX_POINT ( 'NONE', #569 ) ;
#7192 = ADVANCED_FACE ( 'NONE', ( #6122 ), #7502, .F. ) ;
#7193 = DIRECTION ( 'NONE',  ( 0.000000000000000000, 1.000000000000000000, 0.000000000000000000 ) ) ;
#7194 = CARTESIAN_POINT ( 'NONE',  ( -1.044522185028456063, -0.7409939553805848789, 0.006409361585647670688 ) ) ;
#7195 = CALENDAR_DATE ( 2026, 9, 10 ) ;
#7196 = DIRECTION ( 'NONE',  ( -0.7498009116086186143, 0.6531728565937872100, 0.1056589435873571958 ) ) ;
#7197 = ORIENTED_EDGE ( 'NONE', *, *, #1223, .T. ) ;
#7198 = ORIENTED_EDGE ( 'NONE', *, *, #3797, .T. ) ;
#7199 = PLANE ( 'NONE',  #2937 ) ;
#7200 = EDGE_CURVE ( 'NONE', #6242, #2760, #1022, .T. ) ;
#7201 = FACE_OUTER_BOUND ( 'NONE', #6035, .T. ) ;
#7202 = DIRECTION ( 'NONE',  ( -1.000000000000000000, 0.000000000000000000, 0.000000000000000000 ) ) ;
#7203 = CYLINDRICAL_SURFACE ( 'NONE', #3703, 8.573908398499121120 ) ;
#7204 = CARTESIAN_POINT ( 'NONE',  ( 1.846835003037430534, 1.498370261438588313, 0.000000000000000000 ) ) ;
#7205 = ORIENTED_EDGE ( 'NONE', *, *, #6688, .F. ) ;
#7206 = FACE_OUTER_BOUND ( 'NONE', #8053, .T. ) ;
#7207 = DIRECTION ( 'NONE',  ( -1.000000000000000000, 0.000000000000000000, 0.000000000000000000 ) ) ;
#7208 = LINE ( 'NONE', #6598, #1383 ) ;
#7209 = ORIENTED_EDGE ( 'NONE', *, *, #4989, .T. ) ;
#7210 = CARTESIAN_POINT ( 'NONE',  ( 1.466665248995881576, 0.6909135088951512405, -0.1250000000000000000 ) ) ;
#7211 = DIRECTION ( 'NONE',  ( 0.000000000000000000, 1.000000000000000000, -0.000000000000000000 ) ) ;
#7212 = DIRECTION ( 'NONE',  ( 0.000000000000000000, -0.000000000000000000, 1.000000000000000000 ) ) ;
#7213 = PERSON_AND_ORGANIZATION_ROLE ( 'classification_officer' ) ;
#7214 = ORGANIZATION ( 'NAUO-ORG1', 'UNSPECIFIED', 'UNSPECIFIED' ) ;
#7215 = ORIENTED_EDGE ( 'NONE', *, *, #6642, .F. ) ;
#7216 = CARTESIAN_POINT ( 'NONE',  ( -1.723766588794375387, 1.115324847714046497, -0.08100000000000007194 ) ) ;
#7217 = PRODUCT ( 'Cleco, Fastener, Pusher', 'Cleco, Fastener, Pusher', '', ( #431 ) ) ;
#7218 = ORIENTED_EDGE ( 'NONE', *, *, #5839, .F. ) ;
#7219 = ORIENTED_EDGE ( 'NONE', *, *, #2995, .F. ) ;
#7220 = EDGE_LOOP ( 'NONE', ( #4939, #2394, #4911, #5232, #7355, #4080, #6418 ) ) ;
#7221 = DIRECTION ( 'NONE',  ( 1.000000000000000000, 0.000000000000000000, 0.000000000000000000 ) ) ;
#7222 = ORIENTED_EDGE ( 'NONE', *, *, #6600, .F. ) ;
#7223 = FACE_OUTER_BOUND ( 'NONE', #7767, .T. ) ;
#7224 = CARTESIAN_POINT ( 'NONE',  ( -1.040997396242601791, -0.7528336330030669377, 0.03199999999999999373 ) ) ;
#7225 = SECURITY_CLASSIFICATION_LEVEL ( 'unclassified' ) ;
#7226 = CARTESIAN_POINT ( 'NONE',  ( -0.1250000000000000000, 1.530808498934191509E-17, -0.5599999999999999423 ) ) ;
#7227 = EDGE_LOOP ( 'NONE', ( #4727, #5981, #6113, #4015 ) ) ;
#7228 = ORIENTED_EDGE ( 'NONE', *, *, #6150, .F. ) ;
#7229 = AXIS2_PLACEMENT_3D ( 'NONE', #1828, #1398, #4329 ) ;
#7230 = VERTEX_POINT ( 'NONE', #8061 ) ;
#7231 = EDGE_CURVE ( 'NONE', #7797, #3462, #5605, .T. ) ;
#7232 = APPROVAL_PERSON_ORGANIZATION ( #4394, #4952, #6316 ) ;
#7233 = SECURITY_CLASSIFICATION ( '', '', #1132 ) ;
#7234 = EDGE_CURVE ( 'NONE', #5482, #7484, #5624, .T. ) ;
#7235 = CARTESIAN_POINT ( 'NONE',  ( -6.110602001756019419, -1.404684638105634820, 0.3125000000000000000 ) ) ;
#7236 = CIRCLE ( 'NONE', #3567, 0.1100000000000000006 ) ;
#7237 = DIRECTION ( 'NONE',  ( 0.000000000000000000, -0.000000000000000000, 1.000000000000000000 ) ) ;
#7238 = DIRECTION ( 'NONE',  ( -0.000000000000000000, 1.000000000000000000, -0.000000000000000000 ) ) ;
#7239 = CARTESIAN_POINT ( 'NONE',  ( 0.000000000000000000, 1.362500000000000044, 0.000000000000000000 ) ) ;
#7240 = EDGE_LOOP ( 'NONE', ( #6897, #515 ) ) ;
#7241 = FACE_OUTER_BOUND ( 'NONE', #5959, .T. ) ;
#7242 = CARTESIAN_POINT ( 'NONE',  ( 0.1054677083281892608, 0.6124999999999999334, -0.03125000000000000000 ) ) ;
#7243 = EDGE_CURVE ( 'NONE', #6720, #5415, #1679, .T. ) ;
#7244 = CIRCLE ( 'NONE', #6719, 0.1799999999999999933 ) ;
#7245 = ORIENTED_EDGE ( 'NONE', *, *, #5488, .T. ) ;
#7246 = DIRECTION ( 'NONE',  ( 0.000000000000000000, -0.000000000000000000, -1.000000000000000000 ) ) ;
#7247 = PRODUCT_DEFINITION ( 'UNKNOWN', '', #5925, #904 ) ;
#7248 = CARTESIAN_POINT ( 'NONE',  ( 1.640223930642276118, 1.235377681956740803, -0.1039999999999998703 ) ) ;
#7249 = EDGE_CURVE ( 'NONE', #4304, #873, #6265, .T. ) ;
#7250 = AXIS2_PLACEMENT_3D ( 'NONE', #7106, #2196, #6545 ) ;
#7251 = CARTESIAN_POINT ( 'NONE',  ( 0.3566525292043903339, -0.3408511508279103985, 0.03199999999999999373 ) ) ;
#7252 = ORIENTED_EDGE ( 'NONE', *, *, #4532, .F. ) ;
#7253 = CARTESIAN_POINT ( 'NONE',  ( 0.000000000000000000, 0.03125000000000000000, 0.000000000000000000 ) ) ;
#7254 = VECTOR ( 'NONE', #7726, 39.37007874015748854 ) ;
#7255 = CIRCLE ( 'NONE', #5032, 0.1100000000000000006 ) ;
#7256 = CARTESIAN_POINT ( 'NONE',  ( -1.203142842642319188, -0.2081911224984655251, 0.01565206492142497130 ) ) ;
#7257 = CARTESIAN_POINT ( 'NONE',  ( 1.535356550020815947, 1.850327527696066898, -0.01560080253909610672 ) ) ;
#7258 = PERSON_AND_ORGANIZATION_ROLE ( 'design_supplier' ) ;
#7259 = VERTEX_POINT ( 'NONE', #4468 ) ;
#7260 = PLANE ( 'NONE',  #3899 ) ;
#7261 = EDGE_CURVE ( 'NONE', #3669, #5362, #2712, .T. ) ;
#7262 = DIRECTION ( 'NONE',  ( 1.000000000000000000, 0.000000000000000000, 0.000000000000000000 ) ) ;
#7263 = DIRECTION ( 'NONE',  ( -0.9726399823210831741, -0.2323175946639494671, -0.000000000000000000 ) ) ;
#7264 = AXIS2_PLACEMENT_3D ( 'NONE', #6783, #590, #6818 ) ;
#7265 = LINE ( 'NONE', #4968, #3960 ) ;
#7266 = ORIENTED_EDGE ( 'NONE', *, *, #1836, .F. ) ;
#7267 = AXIS2_PLACEMENT_3D ( 'NONE', #3061, #8048, #6826 ) ;
#7268 = ORIENTED_EDGE ( 'NONE', *, *, #6257, .F. ) ;
#7269 = CARTESIAN_POINT ( 'NONE',  ( -0.1255000000000000282, 1.536931732929928570E-17, 0.06199999999999999956 ) ) ;
#7270 = CARTESIAN_POINT ( 'NONE',  ( 0.000000000000000000, -0.03125000000000000000, 0.2896281645421511231 ) ) ;
#7271 = SECURITY_CLASSIFICATION_LEVEL ( 'unclassified' ) ;
#7272 = DIRECTION ( 'NONE',  ( 0.000000000000000000, 0.000000000000000000, -1.000000000000000000 ) ) ;
#7273 = AXIS2_PLACEMENT_3D ( 'NONE', #47, #7589, #6405 ) ;
#7274 = CARTESIAN_POINT ( 'NONE',  ( -1.803041671366327314, 1.104810305277056592, 0.1649762307749162715 ) ) ;
#7275 = VECTOR ( 'NONE', #2221, 39.37007874015748143 ) ;
#7276 = DESIGN_CONTEXT ( 'detailed design', #1541, 'design' ) ;
#7277 = CARTESIAN_POINT ( 'NONE',  ( 1.536996473475150671, 1.850194254988873244, -0.04789697820840163600 ) ) ;
#7278 = COORDINATED_UNIVERSAL_TIME_OFFSET ( 0, 0, .AHEAD. ) ;
#7279 = DIRECTION ( 'NONE',  ( -0.000000000000000000, -0.000000000000000000, -1.000000000000000000 ) ) ;
#7280 = CARTESIAN_POINT ( 'NONE',  ( -0.1250000000000000000, 0.000000000000000000, 0.000000000000000000 ) ) ;
#7281 = EDGE_CURVE ( 'NONE', #1555, #2075, #1276, .T. ) ;
#7282 = ORIENTED_EDGE ( 'NONE', *, *, #1374, .F. ) ;
#7283 = CIRCLE ( 'NONE', #4022, 0.2148203157102361871 ) ;
#7284 = VECTOR ( 'NONE', #2049, 39.37007874015748143 ) ;
#7285 = CARTESIAN_POINT ( 'NONE',  ( 2.204364238465235822E-17, 1.393749999999999822, 0.1799999999999999933 ) ) ;
#7286 = CARTESIAN_POINT ( 'NONE',  ( 1.517943318015056109, 1.875917005398948456, 0.2500000000000000000 ) ) ;
#7287 = AXIS2_PLACEMENT_3D ( 'NONE', #120, #2608, #6967 ) ;
#7288 = AXIS2_PLACEMENT_3D ( 'NONE', #850, #4703, #268 ) ;
#7289 = AXIS2_PLACEMENT_3D ( 'NONE', #1203, #3588, #6861 ) ;
#7290 = CYLINDRICAL_SURFACE ( 'NONE', #4517, 0.2500000000000000555 ) ;
#7291 = CARTESIAN_POINT ( 'NONE',  ( 0.2935750530104211387, 0.05119392622207447063, 0.000000000000000000 ) ) ;
#7292 = ADVANCED_FACE ( 'NONE', ( #4629 ), #1465, .T. ) ;
#7293 = ADVANCED_FACE ( 'NONE', ( #4508 ), #3117, .T. ) ;
#7294 = FACE_OUTER_BOUND ( 'NONE', #6307, .T. ) ;
#7295 = ORIENTED_EDGE ( 'NONE', *, *, #4841, .T. ) ;
#7296 = AXIS2_PLACEMENT_3D ( 'NONE', #5019, #3142, #6301 ) ;
#7297 = CARTESIAN_POINT ( 'NONE',  ( 1.526053023712018897, 1.146155791044123573, 0.1638240367499944894 ) ) ;
#7298 = VECTOR ( 'NONE', #6411, 39.37007874015748143 ) ;
#7299 = APPROVAL ( #1696, 'UNKNOWN' ) ;
#7300 = EDGE_CURVE ( 'NONE', #1921, #4974, #5212, .T. ) ;
#7301 = AXIS2_PLACEMENT_3D ( 'NONE', #245, #4553, #4586 ) ;
#7302 = CARTESIAN_POINT ( 'NONE',  ( 1.082008577330675347, 0.9412886604525910750, -0.3750000000000000555 ) ) ;
#7303 = CIRCLE ( 'NONE', #5862, 0.1250000000000000000 ) ;
#7304 = DIRECTION ( 'NONE',  ( -0.000000000000000000, -0.000000000000000000, 1.000000000000000000 ) ) ;
#7305 = PERSON_AND_ORGANIZATION ( #4735, #6190 ) ;
#7306 = ORIENTED_EDGE ( 'NONE', *, *, #1440, .F. ) ;
#7307 = CARTESIAN_POINT ( 'NONE',  ( 1.877688265130482037, 1.420950500079102286, -0.07807135826935437950 ) ) ;
#7308 = CARTESIAN_POINT ( 'NONE',  ( 5.999999999999997335, -1.164450207299392140E-14, -0.1849999999999999978 ) ) ;
#7309 = CARTESIAN_POINT ( 'NONE',  ( 1.477974616688189968, 1.237804197611785284, 0.2500000000000000000 ) ) ;
#7310 = ORIENTED_EDGE ( 'NONE', *, *, #7149, .T. ) ;
#7311 = ORIENTED_EDGE ( 'NONE', *, *, #1186, .T. ) ;
#7312 = SHAPE_REPRESENTATION_RELATIONSHIP ( 'NONE' , 'NONE' ,  #1942, #7180 ) ;
#7313 = EDGE_LOOP ( 'NONE', ( #316, #3594 ) ) ;
#7314 = CARTESIAN_POINT ( 'NONE',  ( -0.03125000000000000000, 0.000000000000000000, 0.000000000000000000 ) ) ;
#7315 = DIRECTION ( 'NONE',  ( 1.000000000000000000, 0.000000000000000000, -0.000000000000000000 ) ) ;
#7316 = APPROVAL_STATUS ( 'not_yet_approved' ) ;
#7317 = DIRECTION ( 'NONE',  ( 0.9726399823210830631, 0.2323175946639496336, 0.000000000000000000 ) ) ;
#7318 = DIRECTION ( 'NONE',  ( -1.000000000000000000, 0.000000000000000000, 0.000000000000000000 ) ) ;
#7319 = DIRECTION ( 'NONE',  ( 0.000000000000000000, -1.000000000000000000, 0.000000000000000000 ) ) ;
#7320 = CARTESIAN_POINT ( 'NONE',  ( -1.750746777110393282, 1.631196835986985505, 0.3125000000000000000 ) ) ;
#7321 = COORDINATED_UNIVERSAL_TIME_OFFSET ( 0, 0, .AHEAD. ) ;
#7322 = FACE_OUTER_BOUND ( 'NONE', #4467, .T. ) ;
#7323 = CARTESIAN_POINT ( 'NONE',  ( 0.000000000000000000, 1.112500000000000044, -0.1799999999999999933 ) ) ;
#7324 = CARTESIAN_POINT ( 'NONE',  ( 1.508496569261193576, 1.225487632694739037, 0.2349340013801235194 ) ) ;
#7325 = DIRECTION ( 'NONE',  ( 0.000000000000000000, 0.000000000000000000, 1.000000000000000000 ) ) ;
#7326 =( BOUNDED_CURVE ( )  B_SPLINE_CURVE ( 3, ( #2568, #6922, #5148, #5736 ),
 .UNSPECIFIED., .F., .F. ) 
 B_SPLINE_CURVE_WITH_KNOTS ( ( 4, 4 ),
 ( 4.712388980384713655, 6.283185307179586232 ),
 .UNSPECIFIED. ) 
 CURVE ( )  GEOMETRIC_REPRESENTATION_ITEM ( )  RATIONAL_B_SPLINE_CURVE ( ( 1.000000000000000000, 0.8047378541243705996, 0.8047378541243705996, 1.000000000000000000 ) ) 
 REPRESENTATION_ITEM ( '' )  );
#7327 = CARTESIAN_POINT ( 'NONE',  ( 1.142655413120957197, 0.6307864494084283180, 0.2500000000000000000 ) ) ;
#7328 = CARTESIAN_POINT ( 'NONE',  ( 0.000000000000000000, 0.000000000000000000, 0.2500000000000000000 ) ) ;
#7329 = DIRECTION ( 'NONE',  ( -0.000000000000000000, 0.000000000000000000, 1.000000000000000000 ) ) ;
#7330 = EDGE_LOOP ( 'NONE', ( #4651, #6008, #7702, #4266, #7228, #1034 ) ) ;
#7331 = ORIENTED_EDGE ( 'NONE', *, *, #4684, .T. ) ;
#7332 = CARTESIAN_POINT ( 'NONE',  ( -6.163625881728066247, -1.710116247721755522, -0.05999999999999999778 ) ) ;
#7333 = LINE ( 'NONE', #2951, #2942 ) ;
#7334 = DIRECTION ( 'NONE',  ( -0.6568496200222107007, -0.7540216022612863389, 0.000000000000000000 ) ) ;
#7335 = APPROVAL_DATE_TIME ( #4844, #8089 ) ;
#7336 = ORIENTED_EDGE ( 'NONE', *, *, #5550, .T. ) ;
#7337 = DIRECTION ( 'NONE',  ( -0.000000000000000000, -0.000000000000000000, 1.000000000000000000 ) ) ;
#7338 = CARTESIAN_POINT ( 'NONE',  ( 0.000000000000000000, 0.000000000000000000, -0.5599999999999999423 ) ) ;
#7339 = CC_DESIGN_DATE_AND_TIME_ASSIGNMENT ( #3981, #4681, ( #5402 ) ) ;
#7340 = DIRECTION ( 'NONE',  ( -1.000000000000000000, 0.000000000000000000, 0.000000000000000000 ) ) ;
#7341 = ADVANCED_FACE ( 'NONE', ( #2699 ), #5867, .T. ) ;
#7342 = EDGE_CURVE ( 'NONE', #6549, #3726, #2326, .T. ) ;
#7343 = ORIENTED_EDGE ( 'NONE', *, *, #126, .F. ) ;
#7344 =( NAMED_UNIT ( * ) SI_UNIT ( $, .STERADIAN. ) SOLID_ANGLE_UNIT ( ) );
#7345 = ORIENTED_EDGE ( 'NONE', *, *, #7975, .T. ) ;
#7346 = DIRECTION ( 'NONE',  ( 0.000000000000000000, 1.000000000000000000, 0.000000000000000000 ) ) ;
#7347 = CARTESIAN_POINT ( 'NONE',  ( 0.09365290641821995277, -0.4595491472197770766, 0.2255045796716246553 ) ) ;
#7348 = PERSON_AND_ORGANIZATION ( #6782, #3597 ) ;
#7349 = CC_DESIGN_DATE_AND_TIME_ASSIGNMENT ( #2667, #657, ( #7867 ) ) ;
#7350 = CARTESIAN_POINT ( 'NONE',  ( 0.000000000000000000, 0.000000000000000000, 0.1250000000000000000 ) ) ;
#7351 = EDGE_CURVE ( 'NONE', #5067, #3183, #3772, .T. ) ;
#7352 = EDGE_LOOP ( 'NONE', ( #2847, #2867, #1839, #7952 ) ) ;
#7353 = PRODUCT_DEFINITION_SHAPE ( 'NONE', 'NONE',  #8097 ) ;
#7354 = B_SPLINE_CURVE_WITH_KNOTS ( 'NONE', 3,
 ( #1695, #929, #2849, #5358, #2229, #4856, #2346, #1734, #6692, #6085, #7347, #464, #1075, #3579, #5469, #2967, #7956, #2293 ),
 .UNSPECIFIED., .F., .F.,
 ( 4, 2, 2, 2, 2, 2, 2, 2, 4 ),
 ( 0.000000000000000000, 0.0009393808714543294561, 0.001878761742908658912, 0.002818142614362988477, 0.003287833050090153367, 0.003522678267953735162, 0.003640100876885526276, 0.003698812181351423568, 0.003757523485817321294 ),
 .UNSPECIFIED. ) ;
#7355 = ORIENTED_EDGE ( 'NONE', *, *, #3038, .F. ) ;
#7356 = DIRECTION ( 'NONE',  ( 0.6157549048526804736, -0.7879377495398138809, -0.000000000000000000 ) ) ;
#7357 = DIRECTION ( 'NONE',  ( -1.000000000000000000, 0.000000000000000000, 0.000000000000000000 ) ) ;
#7358 = DIRECTION ( 'NONE',  ( 0.000000000000000000, 0.000000000000000000, 1.000000000000000000 ) ) ;
#7359 = APPROVAL_DATE_TIME ( #2351, #4698 ) ;
#7360 = CARTESIAN_POINT ( 'NONE',  ( -0.1250000000000000000, 0.6250000000000000000, 0.03125000000000000000 ) ) ;
#7361 = CARTESIAN_POINT ( 'NONE',  ( -0.1875000000000000278, 0.000000000000000000, 0.06199999999999999956 ) ) ;
#7362 = VECTOR ( 'NONE', #7771, 39.37007874015748143 ) ;
#7363 = ORIENTED_EDGE ( 'NONE', *, *, #6988, .T. ) ;
#7364 = DIRECTION ( 'NONE',  ( 0.000000000000000000, 1.000000000000000000, 0.000000000000000000 ) ) ;
#7365 = DIRECTION ( 'NONE',  ( 9.649454429013021345E-17, 7.540822732871180930E-17, 1.000000000000000000 ) ) ;
#7366 = AXIS2_PLACEMENT_3D ( 'NONE', #1892, #7382, #1157 ) ;
#7367 = CARTESIAN_POINT ( 'NONE',  ( 0.03125000000000000000, -0.03125000000000000000, 0.000000000000000000 ) ) ;
#7368 = CARTESIAN_POINT ( 'NONE',  ( 1.257489209309734290, 1.078422665367065658, -0.07268490389717283118 ) ) ;
#7369 = DIRECTION ( 'NONE',  ( 0.000000000000000000, 1.000000000000000000, 0.000000000000000000 ) ) ;
#7370 = VERTEX_POINT ( 'NONE', #3857 ) ;
#7371 = AXIS2_PLACEMENT_3D ( 'NONE', #3118, #1183, #4960 ) ;
#7372 = ORIENTED_EDGE ( 'NONE', *, *, #3231, .T. ) ;
#7373 = CARTESIAN_POINT ( 'NONE',  ( 1.736793931975229688, 1.310844877195876279, 0.1759093273421855619 ) ) ;
#7374 = AXIS2_PLACEMENT_3D ( 'NONE', #3599, #1056, #7929 ) ;
#7375 = DIRECTION ( 'NONE',  ( 0.6157549048526802515, -0.7879377495398142139, 0.000000000000000000 ) ) ;
#7376 = CARTESIAN_POINT ( 'NONE',  ( 0.000000000000000000, 0.000000000000000000, -0.5599999999999999423 ) ) ;
#7377 = COORDINATED_UNIVERSAL_TIME_OFFSET ( 0, 0, .AHEAD. ) ;
#7378 = ORIENTED_EDGE ( 'NONE', *, *, #1773, .T. ) ;
#7379 = CARTESIAN_POINT ( 'NONE',  ( -1.256933281983527929E-15, 1.050000000000000044, 0.1799999999999999933 ) ) ;
#7380 = DIRECTION ( 'NONE',  ( 0.000000000000000000, 1.000000000000000000, 0.000000000000000000 ) ) ;
#7381 = VERTEX_POINT ( 'NONE', #3973 ) ;
#7382 = DIRECTION ( 'NONE',  ( 0.4964005096718443477, 0.8680936205257663296, -0.000000000000000000 ) ) ;
#7383 = AXIS2_PLACEMENT_3D ( 'NONE', #2162, #6702, #1582 ) ;
#7384 = VECTOR ( 'NONE', #3131, 39.37007874015748143 ) ;
#7385 = VERTEX_POINT ( 'NONE', #7708 ) ;
#7386 = DIRECTION ( 'NONE',  ( -0.2815666759589948720, 0.9595416650617117904, -0.000000000000000000 ) ) ;
#7387 =( CONVERSION_BASED_UNIT ( 'INCH', #5545 ) LENGTH_UNIT ( ) NAMED_UNIT ( #4951 ) );
#7388 = ORIENTED_EDGE ( 'NONE', *, *, #3395, .F. ) ;
#7389 = DIRECTION ( 'NONE',  ( 0.000000000000000000, 0.000000000000000000, -1.000000000000000000 ) ) ;
#7390 = AXIS2_PLACEMENT_3D ( 'NONE', #6661, #5393, #6553 ) ;
#7391 = CARTESIAN_POINT ( 'NONE',  ( 0.000000000000000000, -0.03125000000000000000, 0.6646281645421511231 ) ) ;
#7392 = ADVANCED_FACE ( 'NONE', ( #6394 ), #775, .F. ) ;
#7393 = EDGE_CURVE ( 'NONE', #2877, #141, #4543, .T. ) ;
#7394 = EDGE_CURVE ( 'NONE', #2990, #1116, #3817, .T. ) ;
#7395 = EDGE_LOOP ( 'NONE', ( #7165, #2491, #7071, #999 ) ) ;
#7396 = AXIS2_PLACEMENT_3D ( 'NONE', #7048, #6527, #7175 ) ;
#7397 = EDGE_CURVE ( 'NONE', #4782, #4126, #1256, .T. ) ;
#7398 = ORIENTED_EDGE ( 'NONE', *, *, #4846, .F. ) ;
#7399 = EDGE_CURVE ( 'NONE', #7900, #3851, #2653, .T. ) ;
#7400 = DIRECTION ( 'NONE',  ( 1.000000000000000000, 0.000000000000000000, 0.000000000000000000 ) ) ;
#7401 = CARTESIAN_POINT ( 'NONE',  ( -4.882388066182516084, 5.670153330992327767, -0.05999999999999999778 ) ) ;
#7402 = FACE_OUTER_BOUND ( 'NONE', #4171, .T. ) ;
#7403 = PERSON_AND_ORGANIZATION ( #4735, #6190 ) ;
#7404 = CARTESIAN_POINT ( 'NONE',  ( 0.09374999999999998612, 1.148106374200643401E-17, -0.6537499999999999423 ) ) ;
#7405 = CARTESIAN_POINT ( 'NONE',  ( 0.1054677083281892608, 0.000000000000000000, -0.03125000000000000000 ) ) ;
#7406 = AXIS2_PLACEMENT_3D ( 'NONE', #541, #6258, #5549 ) ;
#7407 = EDGE_LOOP ( 'NONE', ( #4063, #7310, #2569, #6880 ) ) ;
#7408 = CARTESIAN_POINT ( 'NONE',  ( 1.651395268467308108, 1.241511533269027634, 0.1986386654525169326 ) ) ;
#7409 = LINE ( 'NONE', #3681, #1488 ) ;
#7410 = CIRCLE ( 'NONE', #6624, 4.000000000000000888 ) ;
#7411 = DIRECTION ( 'NONE',  ( 0.000000000000000000, 0.000000000000000000, -1.000000000000000000 ) ) ;
#7412 = CARTESIAN_POINT ( 'NONE',  ( -1.723766588794375609, 1.115324847714047385, -0.08100000000000007194 ) ) ;
#7413 = CARTESIAN_POINT ( 'NONE',  ( 6.068104892000603101, -0.009251957739379085624, 0.1250000000000000000 ) ) ;
#7414 = AXIS2_PLACEMENT_3D ( 'NONE', #2899, #6185, #4915 ) ;
#7415 = VERTEX_POINT ( 'NONE', #3317 ) ;
#7416 = EDGE_LOOP ( 'NONE', ( #2494, #2107, #6620, #7188, #3004, #3153, #6686, #6172 ) ) ;
#7417 = CARTESIAN_POINT ( 'NONE',  ( 0.1875000000000000278, 0.000000000000000000, -0.6849999999999999423 ) ) ;
#7418 = CIRCLE ( 'NONE', #7018, 0.2468203157102362155 ) ;
#7419 = AXIS2_PLACEMENT_3D ( 'NONE', #1277, #7468, #8029 ) ;
#7420 = DIRECTION ( 'NONE',  ( 0.7879377495398141029, 0.6157549048526801405, -9.106159978880875423E-16 ) ) ;
#7421 = DIRECTION ( 'NONE',  ( 1.000000000000000000, 0.000000000000000000, -0.000000000000000000 ) ) ;
#7422 = SHAPE_DEFINITION_REPRESENTATION ( #2109, #5024 ) ;
#7423 = ORIENTED_EDGE ( 'NONE', *, *, #2982, .T. ) ;
#7424 = PLANE ( 'NONE',  #1657 ) ;
#7425 = AXIS2_PLACEMENT_3D ( 'NONE', #1373, #1335, #687 ) ;
#7426 = DIRECTION ( 'NONE',  ( -1.000000000000000000, 0.000000000000000000, 0.000000000000000000 ) ) ;
#7427 = ORIENTED_EDGE ( 'NONE', *, *, #7831, .F. ) ;
#7428 = FACE_OUTER_BOUND ( 'NONE', #2247, .T. ) ;
#7429 = AXIS2_PLACEMENT_3D ( 'NONE', #1111, #1719, #5230 ) ;
#7430 = ORIENTED_EDGE ( 'NONE', *, *, #1366, .T. ) ;
#7431 = VECTOR ( 'NONE', #6071, 39.37007874015748143 ) ;
#7432 = ORIENTED_EDGE ( 'NONE', *, *, #3824, .F. ) ;
#7433 = FACE_OUTER_BOUND ( 'NONE', #7923, .T. ) ;
#7434 =( CONVERSION_BASED_UNIT ( 'INCH', #4934 ) LENGTH_UNIT ( ) NAMED_UNIT ( #654 ) );
#7435 = LINE ( 'NONE', #4283, #3191 ) ;
#7436 = ITEM_DEFINED_TRANSFORMATION ( 'NONE', 'NONE', #4479,  #3555 ) ;
#7437 = CARTESIAN_POINT ( 'NONE',  ( -1.042152545007089648, -0.7489535171128813840, 0.2341260034930127132 ) ) ;
#7438 = EDGE_LOOP ( 'NONE', ( #370, #5510, #4845, #5770 ) ) ;
#7439 = EDGE_CURVE ( 'NONE', #713, #2155, #7084, .T. ) ;
#7440 = EDGE_CURVE ( 'NONE', #5561, #5277, #6248, .T. ) ;
#7441 = EDGE_LOOP ( 'NONE', ( #6440, #1801, #4075, #8028, #3135, #6007, #962, #1847 ) ) ;
#7442 = DIRECTION ( 'NONE',  ( -0.000000000000000000, -0.000000000000000000, 1.000000000000000000 ) ) ;
#7443 = DIRECTION ( 'NONE',  ( 1.000000000000000000, 0.000000000000000000, 0.000000000000000000 ) ) ;
#7444 = ADVANCED_FACE ( 'NONE', ( #4028 ), #4672, .F. ) ;
#7445 = DIRECTION ( 'NONE',  ( -1.000000000000000000, 0.000000000000000000, 0.000000000000000000 ) ) ;
#7446 = APPROVAL_STATUS ( 'not_yet_approved' ) ;
#7447 = DIRECTION ( 'NONE',  ( -1.000000000000000000, 0.000000000000000000, 0.000000000000000000 ) ) ;
#7448 = CARTESIAN_POINT ( 'NONE',  ( -0.03921911030312474900, -0.4592703903598064352, 0.000000000000000000 ) ) ;
#7449 = CARTESIAN_POINT ( 'NONE',  ( 1.693003829518198389, 1.370386348581982050, 0.2342090033200751320 ) ) ;
#7450 = CC_DESIGN_PERSON_AND_ORGANIZATION_ASSIGNMENT ( #5998, #4035, ( #7756 ) ) ;
#7451 = ADVANCED_FACE ( 'NONE', ( #283 ), #3408, .F. ) ;
#7452 = ORIENTED_EDGE ( 'NONE', *, *, #7974, .F. ) ;
#7453 = PLANE ( 'NONE',  #6102 ) ;
#7454 = FACE_BOUND ( 'NONE', #7178, .T. ) ;
#7455 = DIRECTION ( 'NONE',  ( 0.000000000000000000, -0.000000000000000000, -1.000000000000000000 ) ) ;
#7456 = ORIENTED_EDGE ( 'NONE', *, *, #1274, .T. ) ;
#7457 = VERTEX_POINT ( 'NONE', #1119 ) ;
#7458 = LINE ( 'NONE', #6153, #7625 ) ;
#7459 = EDGE_CURVE ( 'NONE', #3415, #5374, #6852, .T. ) ;
#7460 = DIRECTION ( 'NONE',  ( -0.000000000000000000, -0.000000000000000000, -1.000000000000000000 ) ) ;
#7461 = CARTESIAN_POINT ( 'NONE',  ( 1.625764008135038186, 1.310881905705549189, 0.2328597852778326871 ) ) ;
#7462 = SECURITY_CLASSIFICATION_LEVEL ( 'unclassified' ) ;
#7463 = ORIENTED_EDGE ( 'NONE', *, *, #4747, .F. ) ;
#7464 = CARTESIAN_POINT ( 'NONE',  ( 1.556400554713971651, 1.293514327272109687, 0.2179999999999999993 ) ) ;
#7465 = CARTESIAN_POINT ( 'NONE',  ( 0.2796912674003787513, -4.528516545235624413, 0.2179999999999999993 ) ) ;
#7466 = EDGE_LOOP ( 'NONE', ( #3965, #6994 ) ) ;
#7467 = CARTESIAN_POINT ( 'NONE',  ( 1.626644885887612135, 1.340816597564956636, 0.2408507084050821034 ) ) ;
#7468 = DIRECTION ( 'NONE',  ( 9.649454429013021345E-17, 7.540822732871180930E-17, 1.000000000000000000 ) ) ;
#7469 = FACE_OUTER_BOUND ( 'NONE', #1605, .T. ) ;
#7470 = DATE_AND_TIME ( #6854, #6227 ) ;
#7471 = DIRECTION ( 'NONE',  ( 0.6157549048526806956, -0.7879377495398136588, 0.000000000000000000 ) ) ;
#7472 = EDGE_LOOP ( 'NONE', ( #3047, #106, #4462, #4875 ) ) ;
#7473 = ORIENTED_EDGE ( 'NONE', *, *, #7459, .F. ) ;
#7474 = PLANE ( 'NONE',  #2704 ) ;
#7475 = CARTESIAN_POINT ( 'NONE',  ( 3.659299226295303686, -8.245510427152350275, -0.1250000000000004441 ) ) ;
#7476 = PERSON_AND_ORGANIZATION ( #4735, #6190 ) ;
#7477 = CARTESIAN_POINT ( 'NONE',  ( -0.9157629057885486867, 0.6051665869063995729, 0.1250000000000000000 ) ) ;
#7478 = CARTESIAN_POINT ( 'NONE',  ( 0.1028096983035134415, -0.4582465879184300372, 0.03199999999999999373 ) ) ;
#7479 = CARTESIAN_POINT ( 'NONE',  ( 0.000000000000000000, 1.112500000000000044, 0.000000000000000000 ) ) ;
#7480 = EDGE_CURVE ( 'NONE', #7825, #2232, #1138, .T. ) ;
#7481 = EDGE_CURVE ( 'NONE', #340, #8047, #2304, .T. ) ;
#7482 = ORIENTED_EDGE ( 'NONE', *, *, #2680, .F. ) ;
#7483 = PRODUCT_DEFINITION_FORMATION_WITH_SPECIFIED_SOURCE ( 'ANY', '', #7672, .NOT_KNOWN. ) ;
#7484 = VERTEX_POINT ( 'NONE', #6289 ) ;
#7485 = AXIS2_PLACEMENT_3D ( 'NONE', #359, #3402, #2769 ) ;
#7486 = PLANE ( 'NONE',  #6752 ) ;
#7487 = CARTESIAN_POINT ( 'NONE',  ( 1.800320205903117809, 1.030513867073702627, -0.1039999999999998703 ) ) ;
#7488 = CARTESIAN_POINT ( 'NONE',  ( 1.475891671935536609, 0.7226544316391472211, 5.393636709996481038 ) ) ;
#7489 = EDGE_CURVE ( 'NONE', #6917, #1875, #7, .T. ) ;
#7490 = ORIENTED_EDGE ( 'NONE', *, *, #133, .T. ) ;
#7491 = ADVANCED_FACE ( 'NONE', ( #2544 ), #2462, .F. ) ;
#7492 = DIRECTION ( 'NONE',  ( 0.000000000000000000, 0.000000000000000000, -1.000000000000000000 ) ) ;
#7493 = ADVANCED_FACE ( 'NONE', ( #3165 ), #5330, .T. ) ;
#7494 = AXIS2_PLACEMENT_3D ( 'NONE', #3867, #3908, #3287 ) ;
#7495 = APPROVAL ( #3141, 'UNSPECIFIED' ) ;
#7496 = EDGE_CURVE ( 'NONE', #4174, #3224, #2185, .T. ) ;
#7497 = CARTESIAN_POINT ( 'NONE',  ( 1.747147036660383401, 1.396167064578475392, 0.1856492696740475179 ) ) ;
#7498 = CARTESIAN_POINT ( 'NONE',  ( 1.258616367985684104, -0.02482036785324303815, 0.1849999999999999978 ) ) ;
#7499 = PERSON_AND_ORGANIZATION_ROLE ( 'design_supplier' ) ;
#7500 = ORIENTED_EDGE ( 'NONE', *, *, #1836, .T. ) ;
#7501 = VECTOR ( 'NONE', #6481, 39.37007874015748143 ) ;
#7502 = PLANE ( 'NONE',  #8067 ) ;
#7503 = LINE ( 'NONE', #6889, #2690 ) ;
#7504 = ORIENTED_EDGE ( 'NONE', *, *, #1236, .T. ) ;
#7505 = CARTESIAN_POINT ( 'NONE',  ( 1.612291730907446929, 1.332246407104009212, 0.2442446905291179859 ) ) ;
#7506 = CIRCLE ( 'NONE', #6325, 0.1875000000000000278 ) ;
#7507 = ORIENTED_EDGE ( 'NONE', *, *, #3344, .F. ) ;
#7508 = DIRECTION ( 'NONE',  ( 1.000000000000000000, 0.000000000000000000, 0.000000000000000000 ) ) ;
#7509 = DIRECTION ( 'NONE',  ( 1.000000000000000000, 0.000000000000000000, 0.000000000000000000 ) ) ;
#7510 = CALENDAR_DATE ( 2026, 9, 10 ) ;
#7511 = DIRECTION ( 'NONE',  ( 0.000000000000000000, 0.000000000000000000, 1.000000000000000000 ) ) ;
#7512 = AXIS2_PLACEMENT_3D ( 'NONE', #6146, #3022, #5521 ) ;
#7513 = AXIS2_PLACEMENT_3D ( 'NONE', #481, #1749, #5441 ) ;
#7514 = VECTOR ( 'NONE', #1944, 39.37007874015748854 ) ;
#7515 = CIRCLE ( 'NONE', #5154, 0.1204106507132265275 ) ;
#7516 = ORIENTED_EDGE ( 'NONE', *, *, #670, .F. ) ;
#7517 = CARTESIAN_POINT ( 'NONE',  ( 1.827130846082144711, 1.523584269423862381, 0.03199999999999999373 ) ) ;
#7518 = PLANE ( 'NONE',  #4897 ) ;
#7519 = APPROVAL_STATUS ( 'not_yet_approved' ) ;
#7520 = LINE ( 'NONE', #5642, #491 ) ;
#7521 = CARTESIAN_POINT ( 'NONE',  ( 1.645591831251460357, 1.707080862284764411, -0.02857125970228467995 ) ) ;
#7522 = ORIENTED_EDGE ( 'NONE', *, *, #1472, .F. ) ;
#7523 = AXIS2_PLACEMENT_3D ( 'NONE', #4865, #476, #18 ) ;
#7524 = VECTOR ( 'NONE', #6095, 39.37007874015748143 ) ;
#7525 = EDGE_LOOP ( 'NONE', ( #6655, #1493, #2177, #5911 ) ) ;
#7526 = AXIS2_PLACEMENT_3D ( 'NONE', #2882, #7317, #7762 ) ;
#7527 = EDGE_CURVE ( 'NONE', #353, #6574, #2498, .T. ) ;
#7528 = CIRCLE ( 'NONE', #6872, 8.633956053943499853 ) ;
#7529 = ORIENTED_EDGE ( 'NONE', *, *, #7630, .T. ) ;
#7530 = DIRECTION ( 'NONE',  ( 0.000000000000000000, 0.000000000000000000, 1.000000000000000000 ) ) ;
#7531 = CARTESIAN_POINT ( 'NONE',  ( 1.415867837616119340, 1.058804471812468062, -0.2073170131698808538 ) ) ;
#7532 = CARTESIAN_POINT ( 'NONE',  ( 0.8923633780935220638, 0.7607014108325284019, 0.2179999999999999993 ) ) ;
#7533 = ORIENTED_EDGE ( 'NONE', *, *, #3791, .F. ) ;
#7534 = DIRECTION ( 'NONE',  ( 0.000000000000000000, 0.000000000000000000, 1.000000000000000000 ) ) ;
#7535 = AXIS2_PLACEMENT_3D ( 'NONE', #4069, #5875, #4717 ) ;
#7536 = EDGE_CURVE ( 'NONE', #6628, #3425, #3784, .T. ) ;
#7537 = EDGE_CURVE ( 'NONE', #3622, #6856, #1239, .T. ) ;
#7538 = PLANE ( 'NONE',  #4399 ) ;
#7539 = CARTESIAN_POINT ( 'NONE',  ( 1.640223930641419914, 1.235377681954054285, -0.08212881570848259982 ) ) ;
#7540 = TOROIDAL_SURFACE ( 'NONE', #78, 0.09374999999999998612, 0.03125000000000000000 ) ;
#7541 = COORDINATED_UNIVERSAL_TIME_OFFSET ( 0, 0, .AHEAD. ) ;
#7542 = ORIENTED_EDGE ( 'NONE', *, *, #6091, .T. ) ;
#7543 = DIRECTION ( 'NONE',  ( -0.000000000000000000, -0.000000000000000000, -1.000000000000000000 ) ) ;
#7544 =( BOUNDED_SURFACE ( )  B_SPLINE_SURFACE ( 3, 2, ( 
 ( #254, #6002, #3451 ),
 ( #3380, #7905, #2799 ),
 ( #2187, #4155, #5347 ),
 ( #5307, #7862, #1001 ),
 ( #7309, #6540, #7794 ),
 ( #7828, #5265, #1528 ),
 ( #4108, #6652, #3417 ),
 ( #4686, #1566, #4070 ) ),
 .UNSPECIFIED., .F., .F., .F. ) 
 B_SPLINE_SURFACE_WITH_KNOTS ( ( 4, 2, 2, 4 ),
 ( 3, 3 ),
 ( 0.000000000000000000, 0.001832226346958918360, 0.002748339520438377540, 0.003664452693917836720 ),
 ( 0.000000000000000000, 1.000000000000000000 ),
 .UNSPECIFIED. ) 
 GEOMETRIC_REPRESENTATION_ITEM ( )  RATIONAL_B_SPLINE_SURFACE ( (
 ( 1.000000000000000000, 0.8944458564818607016, 1.000000000000000000),
 ( 1.000000000000000000, 0.8900330376657383802, 1.000000000000000000),
 ( 1.000000000000000000, 0.8807711115184968520, 1.000000000000000000),
 ( 1.000000000000000000, 0.8564896213547265047, 1.000000000000000000),
 ( 1.000000000000000000, 0.8466679407797762513, 1.000000000000000000),
 ( 1.000000000000000000, 0.8220717958220354893, 1.000000000000000000),
 ( 1.000000000000000000, 0.8073589957100081316, 1.000000000000000000),
 ( 1.000000000000000000, 0.7881701093105710765, 1.000000000000000000) ) ) 
 REPRESENTATION_ITEM ( '' )  SURFACE ( )  );
#7545 = DIRECTION ( 'NONE',  ( 0.000000000000000000, 0.000000000000000000, 1.000000000000000000 ) ) ;
#7546 = AXIS2_PLACEMENT_3D ( 'NONE', #5251, #3522, #2284 ) ;
#7547 = CYLINDRICAL_SURFACE ( 'NONE', #3048, 0.2148203157102362704 ) ;
#7548 = CC_DESIGN_PERSON_AND_ORGANIZATION_ASSIGNMENT ( #7598, #5759, ( #5666 ) ) ;
#7549 = VECTOR ( 'NONE', #2707, 39.37007874015748143 ) ;
#7550 = EDGE_CURVE ( 'NONE', #297, #7167, #8056, .T. ) ;
#7551 = ADVANCED_FACE ( 'NONE', ( #7433 ), #5188, .T. ) ;
#7552 = EDGE_LOOP ( 'NONE', ( #6509, #617, #6666, #6368 ) ) ;
#7553 = TOROIDAL_SURFACE ( 'NONE', #1529, 0.4070000000000000839, 0.03200000000000000067 ) ;
#7554 = CARTESIAN_POINT ( 'NONE',  ( 3.690413561029368683, -8.374393170229348371, 0.1849999999999999978 ) ) ;
#7555 = APPLICATION_PROTOCOL_DEFINITION ( 'international standard', 'config_control_design', 1994, #4314 ) ;
#7556 = DIRECTION ( 'NONE',  ( 0.2323175946639585154, -0.9726399823210809537, 0.000000000000000000 ) ) ;
#7557 = DIRECTION ( 'NONE',  ( -0.7879377495398138809, -0.6157549048526803626, 0.000000000000000000 ) ) ;
#7558 = AXIS2_PLACEMENT_3D ( 'NONE', #7360, #594, #2318 ) ;
#7559 = APPLICATION_CONTEXT ( 'configuration controlled 3d designs of mechanical parts and assemblies' ) ;
#7560 = VECTOR ( 'NONE', #7800, 39.37007874015748143 ) ;
#7561 = ORIENTED_EDGE ( 'NONE', *, *, #5354, .T. ) ;
#7562 = CARTESIAN_POINT ( 'NONE',  ( 0.000000000000000000, 0.03124999999999997571, 0.000000000000000000 ) ) ;
#7563 = DIRECTION ( 'NONE',  ( -0.000000000000000000, -0.000000000000000000, -1.000000000000000000 ) ) ;
#7564 = APPROVAL_DATE_TIME ( #7027, #5598 ) ;
#7565 = DIRECTION ( 'NONE',  ( 1.000000000000000000, 0.000000000000000000, 0.000000000000000000 ) ) ;
#7566 = LINE ( 'NONE', #1492, #2683 ) ;
#7567 = ORIENTED_EDGE ( 'NONE', *, *, #3488, .F. ) ;
#7568 = DIRECTION ( 'NONE',  ( 0.000000000000000000, -0.000000000000000000, 1.000000000000000000 ) ) ;
#7569 = ORIENTED_EDGE ( 'NONE', *, *, #5297, .F. ) ;
#7570 = DIRECTION ( 'NONE',  ( -0.000000000000000000, -0.000000000000000000, -1.000000000000000000 ) ) ;
#7571 = CARTESIAN_POINT ( 'NONE',  ( 0.000000000000000000, 0.000000000000000000, 0.000000000000000000 ) ) ;
#7572 = DIRECTION ( 'NONE',  ( 0.000000000000000000, 0.000000000000000000, 1.000000000000000000 ) ) ;
#7573 = ORIENTED_EDGE ( 'NONE', *, *, #3486, .T. ) ;
#7574 = CARTESIAN_POINT ( 'NONE',  ( 0.1255000000000000282, 0.000000000000000000, 0.06199999999999999956 ) ) ;
#7575 = PERSON ( 'NAUO-PER1', 'UNSPECIFIED', 'UNSPECIFIED', ('UNSPECIFIED'), ('UNSPECIFIED'), ('UNSPECIFIED') ) ;
#7576 = CARTESIAN_POINT ( 'NONE',  ( 0.2896281645421511231, -0.04777128394798136474, 0.000000000000000000 ) ) ;
#7577 = DIRECTION ( 'NONE',  ( -0.6157549048526801405, 0.7879377495398142139, 0.000000000000000000 ) ) ;
#7578 = APPROVAL_DATE_TIME ( #6964, #3146 ) ;
#7579 = ORIENTED_EDGE ( 'NONE', *, *, #5348, .T. ) ;
#7580 = CARTESIAN_POINT ( 'NONE',  ( 0.000000000000000000, 1.050000000000000044, 0.000000000000000000 ) ) ;
#7581 = CARTESIAN_POINT ( 'NONE',  ( 1.356840083662244734, 0.003162463486408387866, 0.1850000000000003586 ) ) ;
#7582 = CARTESIAN_POINT ( 'NONE',  ( 0.1250000000000000278, 0.03125000000000000000, 0.06250000000000000000 ) ) ;
#7583 = EDGE_CURVE ( 'NONE', #3663, #4400, #1772, .T. ) ;
#7584 =( BOUNDED_SURFACE ( )  B_SPLINE_SURFACE ( 3, 2, ( 
 ( #6224, #6823, #1134 ),
 ( #595, #3143, #1169 ),
 ( #1864, #5643, #5020 ),
 ( #4372, #1911, #1207 ),
 ( #6178, #7521, #5516 ),
 ( #5610, #3056, #3104 ),
 ( #4420, #2393, #4294 ),
 ( #7966, #3642, #8085 ) ),
 .UNSPECIFIED., .F., .F., .F. ) 
 B_SPLINE_SURFACE_WITH_KNOTS ( ( 4, 2, 2, 4 ),
 ( 3, 3 ),
 ( 0.01821389010018729937, 0.02536405575626812098, 0.02893913858430853178, 0.03251422141234894259 ),
 ( 0.000000000000000000, 1.000000000000000000 ),
 .UNSPECIFIED. ) 
 GEOMETRIC_REPRESENTATION_ITEM ( )  RATIONAL_B_SPLINE_SURFACE ( (
 ( 1.000000000000000000, 0.9094853233922192137, 1.000000000000000000),
 ( 1.000000000000000000, 0.9206922740272390770, 1.000000000000000000),
 ( 1.000000000000000000, 0.9314353586015322595, 1.000000000000000000),
 ( 1.000000000000000000, 0.9469214819804713246, 1.000000000000000000),
 ( 1.000000000000000000, 0.9519774771984306216, 1.000000000000000000),
 ( 1.000000000000000000, 0.9618860785231415633, 1.000000000000000000),
 ( 1.000000000000000000, 0.9667392787164085233, 1.000000000000000000),
 ( 1.000000000000000000, 0.9714909886463486410, 1.000000000000000000) ) ) 
 REPRESENTATION_ITEM ( '' )  SURFACE ( )  );
#7585 = DIRECTION ( 'NONE',  ( -1.000000000000000000, 0.000000000000000000, 0.000000000000000000 ) ) ;
#7586 =( NAMED_UNIT ( * ) PLANE_ANGLE_UNIT ( ) SI_UNIT ( $, .RADIAN. ) );
#7587 = CARTESIAN_POINT ( 'NONE',  ( 0.3566525292043903339, -0.3408511508279103985, 0.03199999999999999373 ) ) ;
#7588 = EDGE_CURVE ( 'NONE', #5803, #4985, #4932, .T. ) ;
#7589 = DIRECTION ( 'NONE',  ( 0.000000000000000000, 1.000000000000000000, 0.000000000000000000 ) ) ;
#7590 = ORIENTED_EDGE ( 'NONE', *, *, #7595, .T. ) ;
#7591 = EDGE_CURVE ( 'NONE', #898, #6392, #2693, .T. ) ;
#7592 = EDGE_CURVE ( 'NONE', #3346, #4364, #2166, .T. ) ;
#7593 = VERTEX_POINT ( 'NONE', #1310 ) ;
#7594 = PRODUCT_DEFINITION ( 'UNKNOWN', '', #1211, #2857 ) ;
#7595 = EDGE_CURVE ( 'NONE', #6429, #3711, #4802, .T. ) ;
#7596 = DIRECTION ( 'NONE',  ( 0.000000000000000000, 0.000000000000000000, -1.000000000000000000 ) ) ;
#7597 = CYLINDRICAL_SURFACE ( 'NONE', #6379, 0.2148203157102362704 ) ;
#7598 = PERSON_AND_ORGANIZATION ( #4735, #6190 ) ;
#7599 = DIRECTION ( 'NONE',  ( -0.000000000000000000, -0.000000000000000000, 1.000000000000000000 ) ) ;
#7600 = DIRECTION ( 'NONE',  ( 1.000000000000000000, -0.000000000000000000, 1.224646799147353207E-16 ) ) ;
#7601 = ORIENTED_EDGE ( 'NONE', *, *, #7735, .T. ) ;
#7602 = ORIENTED_EDGE ( 'NONE', *, *, #2887, .F. ) ;
#7603 = ORIENTED_EDGE ( 'NONE', *, *, #1879, .T. ) ;
#7604 = CARTESIAN_POINT ( 'NONE',  ( 1.570147038066920908, 1.304011843337828491, 0.2500000000000000000 ) ) ;
#7605 = CARTESIAN_POINT ( 'NONE',  ( 1.389858159471070609, 1.065857478577425521, -0.1776095199200875552 ) ) ;
#7606 = DIRECTION ( 'NONE',  ( -1.000000000000000000, 0.000000000000000000, 0.000000000000000000 ) ) ;
#7607 = CC_DESIGN_SECURITY_CLASSIFICATION ( #5666, ( #4611 ) ) ;
#7608 = DIRECTION ( 'NONE',  ( 0.000000000000000000, 0.000000000000000000, -1.000000000000000000 ) ) ;
#7609 = CARTESIAN_POINT ( 'NONE',  ( 0.1255000000000000282, 0.000000000000000000, 0.1250000000000000000 ) ) ;
#7610 = CC_DESIGN_APPROVAL ( #3996, ( #5651 ) ) ;
#7611 = CARTESIAN_POINT ( 'NONE',  ( 0.000000000000000000, 0.000000000000000000, 0.06300000000000000044 ) ) ;
#7612 = PERSON_AND_ORGANIZATION_ROLE ( 'creator' ) ;
#7613 = ORIENTED_EDGE ( 'NONE', *, *, #829, .T. ) ;
#7614 = CARTESIAN_POINT ( 'NONE',  ( 0.000000000000000000, 0.6124999999999999334, -0.03125000000000000000 ) ) ;
#7615 = DIRECTION ( 'NONE',  ( -0.000000000000000000, -0.000000000000000000, -1.000000000000000000 ) ) ;
#7616 = ORIENTED_EDGE ( 'NONE', *, *, #7002, .F. ) ;
#7617 = AXIS2_PLACEMENT_3D ( 'NONE', #2733, #909, #3922 ) ;
#7618 = CARTESIAN_POINT ( 'NONE',  ( -0.1250000000000000000, 0.000000000000000000, 0.1250000000000000000 ) ) ;
#7619 = VERTEX_POINT ( 'NONE', #790 ) ;
#7620 = LOCAL_TIME ( 14, 45, 32.00000000000000000, #4453 ) ;
#7621 = CARTESIAN_POINT ( 'NONE',  ( 0.000000000000000000, 0.7500000000000001110, -0.1150000000000000050 ) ) ;
#7622 = CARTESIAN_POINT ( 'NONE',  ( -1.424379639128854791, 0.8545203780043559849, -0.1657613293278376587 ) ) ;
#7623 = FACE_OUTER_BOUND ( 'NONE', #271, .T. ) ;
#7624 = CARTESIAN_POINT ( 'NONE',  ( 1.661823184001568698, 1.248966711494948312, 0.1978336168691578745 ) ) ;
#7625 = VECTOR ( 'NONE', #4339, 39.37007874015748854 ) ;
#7626 = ORIENTED_EDGE ( 'NONE', *, *, #29, .F. ) ;
#7627 = ORIENTED_EDGE ( 'NONE', *, *, #2423, .T. ) ;
#7628 = DIRECTION ( 'NONE',  ( 0.000000000000000000, 1.000000000000000000, -0.000000000000000000 ) ) ;
#7629 = EDGE_CURVE ( 'NONE', #6563, #3903, #5199, .T. ) ;
#7630 = EDGE_CURVE ( 'NONE', #2075, #1555, #5589, .T. ) ;
#7631 = CIRCLE ( 'NONE', #564, 8.513908398499120622 ) ;
#7632 = DIRECTION ( 'NONE',  ( -0.000000000000000000, -0.000000000000000000, 1.000000000000000000 ) ) ;
#7633 = SHAPE_DEFINITION_REPRESENTATION ( #7861, #2505 ) ;
#7634 = DIRECTION ( 'NONE',  ( 1.000000000000000000, 0.000000000000000000, 0.000000000000000000 ) ) ;
#7635 = EDGE_CURVE ( 'NONE', #5923, #6844, #1919, .T. ) ;
#7636 = CC_DESIGN_PERSON_AND_ORGANIZATION_ASSIGNMENT ( #890, #7801, ( #2562 ) ) ;
#7637 = EDGE_LOOP ( 'NONE', ( #7650, #4711, #1802, #4298 ) ) ;
#7638 = AXIS2_PLACEMENT_3D ( 'NONE', #1442, #2066, #3870 ) ;
#7639 = EDGE_CURVE ( 'NONE', #1929, #4299, #875, .T. ) ;
#7640 = AXIS2_PLACEMENT_3D ( 'NONE', #6306, #3262, #2074 ) ;
#7641 = ADVANCED_FACE ( 'NONE', ( #7667 ), #1965, .T. ) ;
#7642 = VERTEX_POINT ( 'NONE', #1434 ) ;
#7643 = FACE_OUTER_BOUND ( 'NONE', #1228, .T. ) ;
#7644 = ORIENTED_EDGE ( 'NONE', *, *, #7342, .T. ) ;
#7645 = CARTESIAN_POINT ( 'NONE',  ( -1.855136387357835481, 0.9645206712600612464, -0.08100000000000007194 ) ) ;
#7646 = CARTESIAN_POINT ( 'NONE',  ( 0.000000000000000000, 1.362500000000000044, 0.000000000000000000 ) ) ;
#7647 = ORGANIZATION ( 'NAUO-ORG5', 'UNSPECIFIED', 'UNSPECIFIED' ) ;
#7648 = CIRCLE ( 'NONE', #4910, 0.1100000000000000006 ) ;
#7649 = FACE_OUTER_BOUND ( 'NONE', #1814, .T. ) ;
#7650 = ORIENTED_EDGE ( 'NONE', *, *, #428, .F. ) ;
#7651 = CARTESIAN_POINT ( 'NONE',  ( 0.03125000000000000000, -0.03125000000000000000, 0.1162848326531996240 ) ) ;
#7652 = CLOSED_SHELL ( 'NONE', ( #1678, #2885, #3997, #2572, #319, #633, #2790, #2830, #5092, #3391, #1685, #2189, #5246, #5887, #6743, #4794, #7341, #1181, #7491, #1178, #5647, #2121, #6489, #3748, #4049, #3068, #4491, #2884, #6684, #1325, #5700, #1783, #1971, #5636, #4041, #6106, #4852, #3246, #6649, #6400, #1417, #6558, #1725, #7551, #5827 ) ) ;
#7653 = VECTOR ( 'NONE', #556, 39.37007874015748143 ) ;
#7654 = CARTESIAN_POINT ( 'NONE',  ( 1.824088629755107549, 1.472086675550743129, 0.07316101119560965149 ) ) ;
#7655 = CARTESIAN_POINT ( 'NONE',  ( -1.484384414703910027, 0.9067922411947358929, 0.1720737575213687476 ) ) ;
#7656 = APPROVAL_ROLE ( '' ) ;
#7657 = EDGE_LOOP ( 'NONE', ( #555, #3762, #3876, #5693, #4596, #1968 ) ) ;
#7658 = CARTESIAN_POINT ( 'NONE',  ( 1.244866787915867912, 1.068558539350931369, -0.06210292240210582571 ) ) ;
#7659 = APPLICATION_CONTEXT ( 'configuration controlled 3d designs of mechanical parts and assemblies' ) ;
#7660 = FACE_OUTER_BOUND ( 'NONE', #490, .T. ) ;
#7661 = CIRCLE ( 'NONE', #5176, 8.633956053943499853 ) ;
#7662 = EDGE_LOOP ( 'NONE', ( #201, #5746, #5275, #6706 ) ) ;
#7663 = VERTEX_POINT ( 'NONE', #5220 ) ;
#7664 = LINE ( 'NONE', #2584, #3178 ) ;
#7665 = CIRCLE ( 'NONE', #4138, 0.3243589946935200308 ) ;
#7666 = CARTESIAN_POINT ( 'NONE',  ( 0.000000000000000000, 0.000000000000000000, 0.000000000000000000 ) ) ;
#7667 = FACE_OUTER_BOUND ( 'NONE', #422, .T. ) ;
#7668 = SHAPE_REPRESENTATION_RELATIONSHIP ( 'NONE' , 'NONE' ,  #5024, #1981 ) ;
#7669 = CARTESIAN_POINT ( 'NONE',  ( 0.03125000000000000000, 0.000000000000000000, 0.1162848326531996102 ) ) ;
#7670 = AXIS2_PLACEMENT_3D ( 'NONE', #36, #735, #3236 ) ;
#7671 = CARTESIAN_POINT ( 'NONE',  ( 1.507878486496126325, 1.864120309560733046, -0.0006456303409778649856 ) ) ;
#7672 = PRODUCT ( 'Cleco, Fastener, Center, Split', 'Cleco, Fastener, Center, Split', '', ( #496 ) ) ;
#7673 = CARTESIAN_POINT ( 'NONE',  ( 1.666036690277059584, 1.312801532736543875, 0.1943274194496727170 ) ) ;
#7674 = VECTOR ( 'NONE', #2745, 39.37007874015748143 ) ;
#7675 = CIRCLE ( 'NONE', #1142, 0.1100000000000000006 ) ;
#7676 = VECTOR ( 'NONE', #3664, 39.37007874015748143 ) ;
#7677 = CARTESIAN_POINT ( 'NONE',  ( 3.566133519791359507, 0.3212125039962120954, 0.1250000000000000278 ) ) ;
#7678 = EDGE_LOOP ( 'NONE', ( #2709, #6114 ) ) ;
#7679 = B_SPLINE_CURVE_WITH_KNOTS ( 'NONE', 3,
 ( #2932, #2320, #1704, #4255, #4328, #2475 ),
 .UNSPECIFIED., .F., .F.,
 ( 4, 2, 4 ),
 ( 0.000000000000000000, 0.001832226346962038694, 0.003664452693924077388 ),
 .UNSPECIFIED. ) ;
#7680 = DIRECTION ( 'NONE',  ( -1.000000000000000000, 0.000000000000000000, 0.000000000000000000 ) ) ;
#7681 = CALENDAR_DATE ( 2026, 9, 10 ) ;
#7682 = DIRECTION ( 'NONE',  ( 0.000000000000000000, 0.000000000000000000, 1.000000000000000000 ) ) ;
#7683 = FACE_OUTER_BOUND ( 'NONE', #5127, .T. ) ;
#7684 = EDGE_LOOP ( 'NONE', ( #3998, #3917, #2636, #3465 ) ) ;
#7685 = CIRCLE ( 'NONE', #2315, 0.09904388296398869418 ) ;
#7686 = ORIENTED_EDGE ( 'NONE', *, *, #3885, .T. ) ;
#7687 = EDGE_CURVE ( 'NONE', #2759, #4400, #3862, .T. ) ;
#7688 = EDGE_CURVE ( 'NONE', #4149, #3809, #6361, .T. ) ;
#7689 = ORIENTED_EDGE ( 'NONE', *, *, #1538, .T. ) ;
#7690 = VERTEX_POINT ( 'NONE', #5824 ) ;
#7691 = AXIS2_PLACEMENT_3D ( 'NONE', #618, #4274, #8020 ) ;
#7692 = ORIENTED_EDGE ( 'NONE', *, *, #7550, .F. ) ;
#7693 = AXIS2_PLACEMENT_3D ( 'NONE', #2020, #1361, #3340 ) ;
#7694 = CARTESIAN_POINT ( 'NONE',  ( 1.710665627987878468, 1.385179670250965778, 0.1690855662849976571 ) ) ;
#7695 = EDGE_LOOP ( 'NONE', ( #1259, #2965, #1011, #2609 ) ) ;
#7696 = CARTESIAN_POINT ( 'NONE',  ( 1.669937403698680045, 1.364736155589769462, 0.2262520360130875763 ) ) ;
#7697 = CARTESIAN_POINT ( 'NONE',  ( 1.405770222897310129, 1.058238628546103843, -0.1877720200186123178 ) ) ;
#7698 = CC_DESIGN_DATE_AND_TIME_ASSIGNMENT ( #6196, #7899, ( #3550 ) ) ;
#7699 = EDGE_CURVE ( 'NONE', #305, #6311, #1390, .T. ) ;
#7700 = PLANE ( 'NONE',  #3435 ) ;
#7701 = DIRECTION ( 'NONE',  ( 1.000000000000000000, 0.000000000000000000, -1.224646799147353207E-16 ) ) ;
#7702 = ORIENTED_EDGE ( 'NONE', *, *, #7838, .F. ) ;
#7703 = CARTESIAN_POINT ( 'NONE',  ( 1.455867074896413094, 1.788230745717717340, 0.1579256027718150546 ) ) ;
#7704 = APPROVAL ( #6725, 'UNSPECIFIED' ) ;
#7705 = CARTESIAN_POINT ( 'NONE',  ( 0.1250000000000000278, -0.03125000000000000000, 0.06250000000000000000 ) ) ;
#7706 = PERSON_AND_ORGANIZATION_ROLE ( 'design_owner' ) ;
#7707 = ORIENTED_EDGE ( 'NONE', *, *, #2330, .T. ) ;
#7708 = CARTESIAN_POINT ( 'NONE',  ( 0.1250000000000000278, -0.03125000000000000000, 0.000000000000000000 ) ) ;
#7709 = DIRECTION ( 'NONE',  ( -0.000000000000000000, -1.000000000000000000, -0.000000000000000000 ) ) ;
#7710 = ORIENTED_EDGE ( 'NONE', *, *, #6250, .T. ) ;
#7711 = DIRECTION ( 'NONE',  ( 1.000000000000000000, 0.000000000000000000, 0.000000000000000000 ) ) ;
#7712 = CYLINDRICAL_SURFACE ( 'NONE', #6482, 0.03200000000000003536 ) ;
#7713 = DATE_AND_TIME ( #5873, #817 ) ;
#7714 = EDGE_LOOP ( 'NONE', ( #6171, #6279, #4610, #5961 ) ) ;
#7715 = DIRECTION ( 'NONE',  ( -0.6568496200222107007, -0.7540216022612862279, 0.000000000000000000 ) ) ;
#7716 = PLANE ( 'NONE',  #694 ) ;
#7717 = VERTEX_POINT ( 'NONE', #5748 ) ;
#7718 = DIRECTION ( 'NONE',  ( -0.000000000000000000, 1.000000000000000000, -0.000000000000000000 ) ) ;
#7719 = DATE_TIME_ROLE ( 'creation_date' ) ;
#7720 = DIRECTION ( 'NONE',  ( -0.000000000000000000, -0.000000000000000000, -1.000000000000000000 ) ) ;
#7721 = DIRECTION ( 'NONE',  ( -0.000000000000000000, -0.000000000000000000, -1.000000000000000000 ) ) ;
#7722 = ORIENTED_EDGE ( 'NONE', *, *, #4246, .F. ) ;
#7723 = ORIENTED_EDGE ( 'NONE', *, *, #2038, .T. ) ;
#7724 = DIRECTION ( 'NONE',  ( -1.000000000000000000, 0.000000000000000000, 0.000000000000000000 ) ) ;
#7725 = ORIENTED_EDGE ( 'NONE', *, *, #4190, .T. ) ;
#7726 = DIRECTION ( 'NONE',  ( -0.7540216022612861169, 0.6568496200222107007, 0.000000000000000000 ) ) ;
#7727 = CARTESIAN_POINT ( 'NONE',  ( 1.258616367985684104, -0.02482036785324303815, -0.1849999999999999978 ) ) ;
#7728 = LINE ( 'NONE', #4619, #4748 ) ;
#7729 = ORIENTED_EDGE ( 'NONE', *, *, #906, .T. ) ;
#7730 = LINE ( 'NONE', #4621, #2927 ) ;
#7731 = PRODUCT ( 'Cleco, Handle, Rivet', 'Cleco, Handle, Rivet', '', ( #4186 ) ) ;
#7732 = CARTESIAN_POINT ( 'NONE',  ( 1.320852648564097009, 1.681729342627086732, 0.2439623838516123966 ) ) ;
#7733 = LINE ( 'NONE', #4061, #6764 ) ;
#7734 = APPROVAL_STATUS ( 'not_yet_approved' ) ;
#7735 = EDGE_CURVE ( 'NONE', #24, #409, #2964, .T. ) ;
#7736 = DIRECTION ( 'NONE',  ( 0.7540216022612861169, -0.6568496200222109227, 0.000000000000000000 ) ) ;
#7737 = CARTESIAN_POINT ( 'NONE',  ( 1.316445289774556660, 1.089505585486493455, -0.1209773538345980948 ) ) ;
#7738 = LOCAL_TIME ( 14, 45, 32.00000000000000000, #4640 ) ;
#7739 = CARTESIAN_POINT ( 'NONE',  ( 6.000000000000000888, 0.000000000000000000, 0.1250000000000000000 ) ) ;
#7740 = VERTEX_POINT ( 'NONE', #1393 ) ;
#7741 = EDGE_CURVE ( 'NONE', #1449, #6459, #5718, .T. ) ;
#7742 = CARTESIAN_POINT ( 'NONE',  ( 1.526053023712018897, 1.146155791044123573, 0.1638240367499944894 ) ) ;
#7743 = CC_DESIGN_PERSON_AND_ORGANIZATION_ASSIGNMENT ( #616, #3778, ( #830 ) ) ;
#7744 = EDGE_CURVE ( 'NONE', #3669, #1449, #7023, .T. ) ;
#7745 = DIRECTION ( 'NONE',  ( 1.000000000000000000, 0.000000000000000000, 0.000000000000000000 ) ) ;
#7746 = CARTESIAN_POINT ( 'NONE',  ( 1.389292273488484053, 1.735715544542429933, 0.2499999999999999167 ) ) ;
#7747 = CALENDAR_DATE ( 2026, 9, 10 ) ;
#7748 = ORIENTED_EDGE ( 'NONE', *, *, #3040, .F. ) ;
#7749 = ORIENTED_EDGE ( 'NONE', *, *, #1320, .T. ) ;
#7750 = AXIS2_PLACEMENT_3D ( 'NONE', #489, #7971, #4873 ) ;
#7751 = ORIENTED_EDGE ( 'NONE', *, *, #7688, .T. ) ;
#7752 = FACE_OUTER_BOUND ( 'NONE', #3616, .T. ) ;
#7753 = CARTESIAN_POINT ( 'NONE',  ( 1.321981203096655788, -0.006563399200562533738, -0.1250000000000000278 ) ) ;
#7754 = LOCAL_TIME ( 14, 45, 32.00000000000000000, #137 ) ;
#7755 = AXIS2_PLACEMENT_3D ( 'NONE', #866, #5946, #325 ) ;
#7756 = PRODUCT_DEFINITION_FORMATION_WITH_SPECIFIED_SOURCE ( 'ANY', '', #795, .NOT_KNOWN. ) ;
#7757 = SHAPE_REPRESENTATION_RELATIONSHIP ( 'NONE' , 'NONE' ,  #6436, #5336 ) ;
#7758 = LINE ( 'NONE', #2848, #43 ) ;
#7759 = CARTESIAN_POINT ( 'NONE',  ( -1.050138139902704104, -0.7221301030214424266, 0.000000000000000000 ) ) ;
#7760 = PERSON_AND_ORGANIZATION ( #7575, #7214 ) ;
#7761 = CARTESIAN_POINT ( 'NONE',  ( 6.191327929239392347, 0.4578608198540764507, 0.000000000000000000 ) ) ;
#7762 = DIRECTION ( 'NONE',  ( -0.2323175946639494671, 0.9726399823210830631, 0.000000000000000000 ) ) ;
#7763 = VECTOR ( 'NONE', #4633, 39.37007874015748143 ) ;
#7764 = VERTEX_POINT ( 'NONE', #3376 ) ;
#7765 = ORIENTED_EDGE ( 'NONE', *, *, #3028, .T. ) ;
#7766 = VERTEX_POINT ( 'NONE', #165 ) ;
#7767 = EDGE_LOOP ( 'NONE', ( #2784, #5094, #129, #1121 ) ) ;
#7768 = CARTESIAN_POINT ( 'NONE',  ( 0.000000000000000000, 0.000000000000000000, 0.000000000000000000 ) ) ;
#7769 = DIRECTION ( 'NONE',  ( -0.7879377495398138809, -0.6157549048526804736, 0.000000000000000000 ) ) ;
#7770 = CARTESIAN_POINT ( 'NONE',  ( 1.240314151020239564, 1.658956310969643022, 0.2179999999999999993 ) ) ;
#7771 = DIRECTION ( 'NONE',  ( -0.000000000000000000, -0.000000000000000000, -1.000000000000000000 ) ) ;
#7772 = CIRCLE ( 'NONE', #4245, 0.2499999999999986955 ) ;
#7773 = AXIS2_PLACEMENT_3D ( 'NONE', #4855, #7346, #6737 ) ;
#7774 = PLANE ( 'NONE',  #2652 ) ;
#7775 = ORIENTED_EDGE ( 'NONE', *, *, #2736, .F. ) ;
#7776 = APPROVAL_PERSON_ORGANIZATION ( #5672, #4489, #3787 ) ;
#7777 = AXIS2_PLACEMENT_3D ( 'NONE', #4204, #8077, #5474 ) ;
#7778 = CARTESIAN_POINT ( 'NONE',  ( 1.349372409038269716, 1.744182786447574296, 0.1909097557292625813 ) ) ;
#7779 = CYLINDRICAL_SURFACE ( 'NONE', #3361, 9.124497838702110286 ) ;
#7780 = DIRECTION ( 'NONE',  ( 0.7879377495398137699, 0.6157549048526805846, 0.000000000000000000 ) ) ;
#7781 = CARTESIAN_POINT ( 'NONE',  ( 6.067385397437120353, 0.2407432673787524013, -0.1250000000000000000 ) ) ;
#7782 = VERTEX_POINT ( 'NONE', #820 ) ;
#7783 = CARTESIAN_POINT ( 'NONE',  ( 1.363867297305675796, 1.069133023682674377, -0.1341576936804522446 ) ) ;
#7784 = TOROIDAL_SURFACE ( 'NONE', #3078, 0.2112499999999999933, 0.03125000000000000000 ) ;
#7785 = EDGE_CURVE ( 'NONE', #5686, #1539, #5259, .T. ) ;
#7786 = EDGE_CURVE ( 'NONE', #1048, #7184, #4766, .T. ) ;
#7787 = FACE_OUTER_BOUND ( 'NONE', #3892, .T. ) ;
#7788 = CARTESIAN_POINT ( 'NONE',  ( 1.437142212823555587, 1.212327995211809117, 0.2500000000000000000 ) ) ;
#7789 = CIRCLE ( 'NONE', #1912, 8.696493751522730520 ) ;
#7790 = SECURITY_CLASSIFICATION_LEVEL ( 'unclassified' ) ;
#7791 = ORIENTED_EDGE ( 'NONE', *, *, #4988, .F. ) ;
#7792 = VECTOR ( 'NONE', #6662, 39.37007874015748143 ) ;
#7793 = DIRECTION ( 'NONE',  ( -1.000000000000000000, 0.000000000000000000, 0.000000000000000000 ) ) ;
#7794 = CARTESIAN_POINT ( 'NONE',  ( 1.493916101511090444, 1.213727529553185303, 0.2318685029578917700 ) ) ;
#7795 = AXIS2_PLACEMENT_3D ( 'NONE', #7338, #6075, #6728 ) ;
#7796 = EDGE_CURVE ( 'NONE', #2606, #7740, #612, .T. ) ;
#7797 = VERTEX_POINT ( 'NONE', #5872 ) ;
#7798 = ORIENTED_EDGE ( 'NONE', *, *, #3925, .F. ) ;
#7799 = CARTESIAN_POINT ( 'NONE',  ( -4.790174522854136363, -3.094341753229061798, 0.2179999999999999993 ) ) ;
#7800 = DIRECTION ( 'NONE',  ( -0.4606913525677331367, -0.8875604078987031631, -0.000000000000000000 ) ) ;
#7801 = PERSON_AND_ORGANIZATION_ROLE ( 'classification_officer' ) ;
#7802 = CARTESIAN_POINT ( 'NONE',  ( -1.855136387357835481, 0.9645206712600612464, -0.2959999999999997078 ) ) ;
#7803 = CIRCLE ( 'NONE', #4278, 4.032000000000000917 ) ;
#7804 = ORIENTED_EDGE ( 'NONE', *, *, #1291, .T. ) ;
#7805 = CIRCLE ( 'NONE', #6508, 0.4070000000000000839 ) ;
#7806 = ORIENTED_EDGE ( 'NONE', *, *, #2742, .F. ) ;
#7807 = AXIS2_PLACEMENT_3D ( 'NONE', #44, #628, #1937 ) ;
#7808 = ORIENTED_EDGE ( 'NONE', *, *, #2587, .F. ) ;
#7809 = CARTESIAN_POINT ( 'NONE',  ( 0.000000000000000000, -0.03125000000000000000, 0.2896281645421511231 ) ) ;
#7811 = CARTESIAN_POINT ( 'NONE',  ( -0.9142296270274463676, 0.5739542246721696106, 0.09374999999999998612 ) ) ;
#7810 = AXIS2_PLACEMENT_3D ( 'NONE', #2567, #5075, #4497 ) ;
#7812 = DIRECTION ( 'NONE',  ( 0.000000000000000000, 0.000000000000000000, 1.000000000000000000 ) ) ;
#7813 = DIRECTION ( 'NONE',  ( -1.000000000000000000, 0.000000000000000000, 0.000000000000000000 ) ) ;
#7814 = CARTESIAN_POINT ( 'NONE',  ( 0.000000000000000000, 0.000000000000000000, -0.1799999999999999933 ) ) ;
#7815 = VECTOR ( 'NONE', #4419, 39.37007874015748854 ) ;
#7816 = EDGE_LOOP ( 'NONE', ( #4866, #5013, #4808, #4924 ) ) ;
#7817 = DIRECTION ( 'NONE',  ( -0.000000000000000000, -1.000000000000000000, -0.000000000000000000 ) ) ;
#7818 = CARTESIAN_POINT ( 'NONE',  ( 0.8135394388129588705, 1.284829519251779573, 0.03200000000000000067 ) ) ;
#7819 = DIRECTION ( 'NONE',  ( 1.000000000000000000, 0.000000000000000000, 0.000000000000000000 ) ) ;
#7820 = EDGE_LOOP ( 'NONE', ( #2072, #3558, #3199, #7372, #3299, #6916 ) ) ;
#7821 = CYLINDRICAL_SURFACE ( 'NONE', #1737, 0.1100000000000000006 ) ;
#7822 = DIRECTION ( 'NONE',  ( 0.000000000000000000, -0.000000000000000000, 1.000000000000000000 ) ) ;
#7823 = FACE_OUTER_BOUND ( 'NONE', #3796, .T. ) ;
#7824 = COORDINATED_UNIVERSAL_TIME_OFFSET ( 0, 0, .AHEAD. ) ;
#7825 = VERTEX_POINT ( 'NONE', #4367 ) ;
#7826 = CARTESIAN_POINT ( 'NONE',  ( 0.000000000000000000, 0.000000000000000000, 0.000000000000000000 ) ) ;
#7827 = EDGE_CURVE ( 'NONE', #4569, #5116, #605, .T. ) ;
#7828 = CARTESIAN_POINT ( 'NONE',  ( 1.457766515874196811, 1.224760407095971892, 0.2500000000000000000 ) ) ;
#7829 = ORIENTED_EDGE ( 'NONE', *, *, #5991, .F. ) ;
#7830 = ORIENTED_EDGE ( 'NONE', *, *, #2521, .T. ) ;
#7831 = EDGE_CURVE ( 'NONE', #225, #3595, #485, .T. ) ;
#7832 = ORIENTED_EDGE ( 'NONE', *, *, #6143, .T. ) ;
#7833 = DIRECTION ( 'NONE',  ( -0.6157549048526729241, 0.7879377495398196540, 0.000000000000000000 ) ) ;
#7834 = DIRECTION ( 'NONE',  ( -6.975840231036812635E-15, -1.000000000000000000, 2.013666839457971600E-30 ) ) ;
#7835 = CONTEXT_DEPENDENT_SHAPE_REPRESENTATION ( #275, #4731 ) ;
#7836 = DIRECTION ( 'NONE',  ( 0.000000000000000000, 0.000000000000000000, -1.000000000000000000 ) ) ;
#7837 = ADVANCED_FACE ( 'NONE', ( #2471 ), #1741, .F. ) ;
#7838 = EDGE_CURVE ( 'NONE', #2698, #7979, #4549, .T. ) ;
#7839 = ORIENTED_EDGE ( 'NONE', *, *, #6093, .T. ) ;
#7840 = VERTEX_POINT ( 'NONE', #2974 ) ;
#7841 = EDGE_CURVE ( 'NONE', #7230, #502, #6784, .T. ) ;
#7842 = VERTEX_POINT ( 'NONE', #472 ) ;
#7843 = CC_DESIGN_PERSON_AND_ORGANIZATION_ASSIGNMENT ( #5579, #7499, ( #4603 ) ) ;
#7844 = EDGE_CURVE ( 'NONE', #1913, #661, #1782, .T. ) ;
#7845 = CARTESIAN_POINT ( 'NONE',  ( -6.057578121783967262, -1.099253028489540318, -0.05999999999999999778 ) ) ;
#7846 = CARTESIAN_POINT ( 'NONE',  ( 0.1250000000000000278, -0.03125000000000000000, 0.000000000000000000 ) ) ;
#7847 = CARTESIAN_POINT ( 'NONE',  ( -6.163625881728066247, -1.710116247721755522, 0.3125000000000000000 ) ) ;
#7848 = CARTESIAN_POINT ( 'NONE',  ( -1.410683006424825692, 0.8425888524880515984, 0.2499905547878000789 ) ) ;
#7849 = DIRECTION ( 'NONE',  ( 0.6424495419751342640, 0.000000000000000000, 0.7663279885375060552 ) ) ;
#7850 = ORIENTED_EDGE ( 'NONE', *, *, #1978, .T. ) ;
#7851 = DIRECTION ( 'NONE',  ( -0.000000000000000000, -0.000000000000000000, -1.000000000000000000 ) ) ;
#7852 = CARTESIAN_POINT ( 'NONE',  ( -1.332203854133312548, 0.7742234353597469143, -0.1918577977169502180 ) ) ;
#7853 = CARTESIAN_POINT ( 'NONE',  ( -0.1250000000000000000, 0.5625000000000000000, -0.03125000000000000000 ) ) ;
#7854 = ORIENTED_EDGE ( 'NONE', *, *, #5488, .F. ) ;
#7855 = CARTESIAN_POINT ( 'NONE',  ( 6.067840808230170246, 0.2405569712445295161, 0.1850000000000003586 ) ) ;
#7856 = CARTESIAN_POINT ( 'NONE',  ( 1.142655413120957197, 0.6307864494084283180, 0.2179999999999999993 ) ) ;
#7857 = CARTESIAN_POINT ( 'NONE',  ( 1.535624491898250898, 1.849481840152294998, -0.03984540547275473854 ) ) ;
#7858 = APPROVAL_DATE_TIME ( #6804, #3935 ) ;
#7859 = ORIENTED_EDGE ( 'NONE', *, *, #7439, .T. ) ;
#7860 = CARTESIAN_POINT ( 'NONE',  ( 1.491488457038117721, 1.855243150880289349, -0.01042660034413028965 ) ) ;
#7861 = PRODUCT_DEFINITION_SHAPE ( 'NONE', 'NONE',  #7594 ) ;
#7862 = CARTESIAN_POINT ( 'NONE',  ( 1.498670457054695593, 1.228438162154884994, 0.2499999999999999722 ) ) ;
#7863 = EDGE_LOOP ( 'NONE', ( #5370, #3334 ) ) ;
#7864 = ORIENTED_EDGE ( 'NONE', *, *, #2587, .T. ) ;
#7865 = CARTESIAN_POINT ( 'NONE',  ( 1.860542729474518930, 1.462361520562285744, -0.01844159883874913960 ) ) ;
#7866 = CARTESIAN_POINT ( 'NONE',  ( 1.398758354407434235, 1.188821195468423131, 0.2500000000000000000 ) ) ;
#7867 = SECURITY_CLASSIFICATION ( '', '', #7462 ) ;
#7868 = CONTEXT_DEPENDENT_SHAPE_REPRESENTATION ( #2794, #5331 ) ;
#7869 = FACE_OUTER_BOUND ( 'NONE', #953, .T. ) ;
#7870 = ORIENTED_EDGE ( 'NONE', *, *, #1184, .F. ) ;
#7871 = CIRCLE ( 'NONE', #685, 0.03125000000000000694 ) ;
#7872 = LOCAL_TIME ( 14, 45, 32.00000000000000000, #821 ) ;
#7873 = CC_DESIGN_APPROVAL ( #5548, ( #1471 ) ) ;
#7874 = ORIENTED_EDGE ( 'NONE', *, *, #1039, .T. ) ;
#7875 = EDGE_CURVE ( 'NONE', #6943, #518, #2435, .T. ) ;
#7876 = LINE ( 'NONE', #2269, #3332 ) ;
#7877 = VECTOR ( 'NONE', #3904, 39.37007874015748854 ) ;
#7878 = CARTESIAN_POINT ( 'NONE',  ( -0.1250000000000000000, 0.6250000000000000000, -0.03125000000000000000 ) ) ;
#7879 = PERSON_AND_ORGANIZATION ( #4735, #6190 ) ;
#7880 = DIRECTION ( 'NONE',  ( 0.6568496200222107007, 0.7540216022612862279, 0.000000000000000000 ) ) ;
#7881 = ORIENTED_EDGE ( 'NONE', *, *, #125, .F. ) ;
#7882 = ORIENTED_EDGE ( 'NONE', *, *, #7090, .T. ) ;
#7883 = CYLINDRICAL_SURFACE ( 'NONE', #5274, 0.1249999999999998473 ) ;
#7884 = ADVANCED_FACE ( 'NONE', ( #5604 ), #7474, .T. ) ;
#7885 = LINE ( 'NONE', #517, #5023 ) ;
#7886 = AXIS2_PLACEMENT_3D ( 'NONE', #941, #5812, #4745 ) ;
#7887 = ORIENTED_EDGE ( 'NONE', *, *, #2188, .T. ) ;
#7888 = ORIENTED_EDGE ( 'NONE', *, *, #5248, .T. ) ;
#7889 = CARTESIAN_POINT ( 'NONE',  ( 0.000000000000000000, 0.000000000000000000, -0.6849999999999999423 ) ) ;
#7890 = DIRECTION ( 'NONE',  ( 0.2873478855663426645, -0.000000000000000000, -0.9578262852211522071 ) ) ;
#7891 = TOROIDAL_SURFACE ( 'NONE', #4765, 0.2112499999999999933, 0.03125000000000000000 ) ;
#7892 = CARTESIAN_POINT ( 'NONE',  ( 0.1250000000000000000, 0.5625000000000000000, -0.03125000000000000000 ) ) ;
#7893 = EDGE_LOOP ( 'NONE', ( #3149, #1073, #1094, #7533 ) ) ;
#7894 = DIRECTION ( 'NONE',  ( 0.000000000000000000, -0.000000000000000000, 1.000000000000000000 ) ) ;
#7895 = CIRCLE ( 'NONE', #6472, 0.09374999999999998612 ) ;
#7896 = VECTOR ( 'NONE', #3822, 39.37007874015748143 ) ;
#7897 = DIRECTION ( 'NONE',  ( -0.9987955914953421388, -0.04906492035527377366, 0.000000000000000000 ) ) ;
#7898 = FACE_OUTER_BOUND ( 'NONE', #7552, .T. ) ;
#7899 = DATE_TIME_ROLE ( 'classification_date' ) ;
#7900 = VERTEX_POINT ( 'NONE', #6096 ) ;
#7901 = DIRECTION ( 'NONE',  ( 0.6568496200222107007, 0.7540216022612862279, -0.000000000000000000 ) ) ;
#7902 = CARTESIAN_POINT ( 'NONE',  ( -0.09374999999999998612, 0.000000000000000000, -0.6849999999999999423 ) ) ;
#7903 = CIRCLE ( 'NONE', #3331, 0.1255000000000000282 ) ;
#7904 = APPROVAL_PERSON_ORGANIZATION ( #890, #2789, #4773 ) ;
#7905 = CARTESIAN_POINT ( 'NONE',  ( 1.546772504294347428, 1.265727676674507585, 0.2500000000000104916 ) ) ;
#7906 = VERTEX_POINT ( 'NONE', #1130 ) ;
#7907 = AXIS2_PLACEMENT_3D ( 'NONE', #3563, #7211, #3612 ) ;
#7908 = ORIENTED_EDGE ( 'NONE', *, *, #6156, .F. ) ;
#7909 = DIRECTION ( 'NONE',  ( 0.000000000000000000, 0.000000000000000000, 1.000000000000000000 ) ) ;
#7910 = FACE_OUTER_BOUND ( 'NONE', #2900, .T. ) ;
#7911 = PERSON_AND_ORGANIZATION_ROLE ( 'classification_officer' ) ;
#7912 = CARTESIAN_POINT ( 'NONE',  ( 1.408343819019455843E-17, 0.7500000000000001110, 0.1150000000000000050 ) ) ;
#7913 = VECTOR ( 'NONE', #221, 39.37007874015748143 ) ;
#7914 = ORIENTED_EDGE ( 'NONE', *, *, #5386, .T. ) ;
#7915 = DIRECTION ( 'NONE',  ( 0.8680936205257663296, -0.4964005096718443477, 0.000000000000000000 ) ) ;
#7916 = AXIS2_PLACEMENT_3D ( 'NONE', #750, #6937, #5782 ) ;
#7917 = DIRECTION ( 'NONE',  ( 0.000000000000000000, 0.000000000000000000, 1.000000000000000000 ) ) ;
#7918 = APPROVAL_PERSON_ORGANIZATION ( #5882, #6687, #6579 ) ;
#7919 = CYLINDRICAL_SURFACE ( 'NONE', #4634, 8.633956053943499853 ) ;
#7920 = APPLICATION_PROTOCOL_DEFINITION ( 'international standard', 'config_control_design', 1994, #5574 ) ;
#7921 = CARTESIAN_POINT ( 'NONE',  ( 4.013019369095008670, -4.147396371033809537, -0.1250000000000000000 ) ) ;
#7922 = CARTESIAN_POINT ( 'NONE',  ( 0.000000000000000000, 0.000000000000000000, -0.1799999999999999933 ) ) ;
#7923 = EDGE_LOOP ( 'NONE', ( #2332, #2670, #1209, #1530 ) ) ;
#7924 = AXIS2_PLACEMENT_3D ( 'NONE', #4752, #6596, #5940 ) ;
#7925 = AXIS2_PLACEMENT_3D ( 'NONE', #3326, #4560, #3206 ) ;
#7926 = EDGE_CURVE ( 'NONE', #1110, #1684, #1661, .T. ) ;
#7927 = CARTESIAN_POINT ( 'NONE',  ( 1.551450996633589874, 1.150725612071006987, 0.1733116977521490798 ) ) ;
#7928 = EDGE_CURVE ( 'NONE', #4493, #4174, #745, .T. ) ;
#7929 = DIRECTION ( 'NONE',  ( 0.7879377495398139919, 0.6157549048526803626, 0.000000000000000000 ) ) ;
#7930 = ADVANCED_FACE ( 'NONE', ( #6746 ), #2314, .T. ) ;
#7931 = VECTOR ( 'NONE', #6822, 39.37007874015748143 ) ;
#7932 = AXIS2_PLACEMENT_3D ( 'NONE', #3013, #591, #5512 ) ;
#7933 = CC_DESIGN_PERSON_AND_ORGANIZATION_ASSIGNMENT ( #4595, #369, ( #6001 ) ) ;
#7934 = CARTESIAN_POINT ( 'NONE',  ( 1.472069962421740819, 0.7095069109563471033, 0.1250000000000000000 ) ) ;
#7935 = ADVANCED_FACE ( 'NONE', ( #510 ), #4423, .T. ) ;
#7936 = FACE_OUTER_BOUND ( 'NONE', #145, .T. ) ;
#7937 = LINE ( 'NONE', #1800, #6251 ) ;
#7938 = EDGE_CURVE ( 'NONE', #502, #4907, #4205, .T. ) ;
#7939 = ORIENTED_EDGE ( 'NONE', *, *, #3398, .F. ) ;
#7940 = AXIS2_PLACEMENT_3D ( 'NONE', #4762, #4150, #1035 ) ;
#7941 = DIRECTION ( 'NONE',  ( -1.000000000000000000, 0.000000000000000000, 0.000000000000000000 ) ) ;
#7942 = CC_DESIGN_DATE_AND_TIME_ASSIGNMENT ( #3758, #3591, ( #7594 ) ) ;
#7943 = ADVANCED_FACE ( 'NONE', ( #4977 ), #7998, .F. ) ;
#7944 = CARTESIAN_POINT ( 'NONE',  ( 6.317381622560545473, 0.2407432673787524013, -0.1250000000000000000 ) ) ;
#7945 = DIRECTION ( 'NONE',  ( -0.000000000000000000, -0.000000000000000000, -1.000000000000000000 ) ) ;
#7946 = COORDINATED_UNIVERSAL_TIME_OFFSET ( 0, 0, .AHEAD. ) ;
#7947 = ORIENTED_EDGE ( 'NONE', *, *, #1080, .T. ) ;
#7948 = CARTESIAN_POINT ( 'NONE',  ( -4.882388066182508091, 5.670153330992292240, 0.2500000000000000000 ) ) ;
#7949 = PLANE ( 'NONE',  #2425 ) ;
#7950 = CARTESIAN_POINT ( 'NONE',  ( -0.1250000000000000000, 0.5625000000000000000, 0.03125000000000000000 ) ) ;
#7951 = ORIENTED_EDGE ( 'NONE', *, *, #6337, .T. ) ;
#7952 = ORIENTED_EDGE ( 'NONE', *, *, #270, .T. ) ;
#7953 = SHAPE_REPRESENTATION_RELATIONSHIP ( 'NONE' , 'NONE' ,  #2774, #3853 ) ;
#7954 = ORIENTED_EDGE ( 'NONE', *, *, #6683, .T. ) ;
#7955 = PLANE ( 'NONE',  #4376 ) ;
#7956 = CARTESIAN_POINT ( 'NONE',  ( 0.1028096983035128309, -0.4582465879184304258, 0.2187868247782020770 ) ) ;
#7957 = DATE_TIME_ROLE ( 'classification_date' ) ;
#7958 = PLANE ( 'NONE',  #2822 ) ;
#7959 = ORIENTED_EDGE ( 'NONE', *, *, #1141, .F. ) ;
#7960 = ORIENTED_EDGE ( 'NONE', *, *, #5837, .T. ) ;
#7961 = CARTESIAN_POINT ( 'NONE',  ( 0.6597999294535048520, -0.01652128394798136821, 0.07449999999999999678 ) ) ;
#7962 = CARTESIAN_POINT ( 'NONE',  ( 0.000000000000000000, 0.000000000000000000, -0.6537499999999999423 ) ) ;
#7963 = CYLINDRICAL_SURFACE ( 'NONE', #2803, 0.3750000000000000555 ) ;
#7964 = COORDINATED_UNIVERSAL_TIME_OFFSET ( 0, 0, .AHEAD. ) ;
#7965 = DIRECTION ( 'NONE',  ( 0.6157549048526801405, -0.7879377495398139919, 0.000000000000000000 ) ) ;
#7966 = CARTESIAN_POINT ( 'NONE',  ( 1.535739741337429853, 1.855487842895053419, -3.030643867971292100E-16 ) ) ;
#7967 = ORIENTED_EDGE ( 'NONE', *, *, #4388, .F. ) ;
#7968 = CARTESIAN_POINT ( 'NONE',  ( 0.2386870781737283065, -0.03125000000000000000, 0.07449999999999999678 ) ) ;
#7969 = ORIENTED_EDGE ( 'NONE', *, *, #2144, .T. ) ;
#7970 = DIRECTION ( 'NONE',  ( 0.000000000000000000, 0.000000000000000000, -1.000000000000000000 ) ) ;
#7971 = DIRECTION ( 'NONE',  ( 0.000000000000000000, 1.000000000000000000, 0.000000000000000000 ) ) ;
#7972 = ORIENTED_EDGE ( 'NONE', *, *, #5383, .T. ) ;
#7973 = LINE ( 'NONE', #2403, #6977 ) ;
#7974 = EDGE_CURVE ( 'NONE', #4612, #7782, #5728, .T. ) ;
#7975 = EDGE_CURVE ( 'NONE', #255, #646, #3764, .T. ) ;
#7976 = CARTESIAN_POINT ( 'NONE',  ( 1.302790242782180918, 1.667167568704493341, -0.1039999999999998703 ) ) ;
#7977 = FACE_OUTER_BOUND ( 'NONE', #2375, .T. ) ;
#7978 = PERSON_AND_ORGANIZATION ( #4735, #6190 ) ;
#7979 = VERTEX_POINT ( 'NONE', #4942 ) ;
#7980 = EDGE_CURVE ( 'NONE', #668, #3809, #5069, .T. ) ;
#7981 = LINE ( 'NONE', #4310, #6260 ) ;
#7982 = LINE ( 'NONE', #1721, #5322 ) ;
#7983 = VERTEX_POINT ( 'NONE', #5015 ) ;
#7984 = CARTESIAN_POINT ( 'NONE',  ( -1.983451234524918227, 1.341543513548240529, -0.2959999999999997078 ) ) ;
#7985 = EDGE_CURVE ( 'NONE', #477, #1252, #2018, .T. ) ;
#7986 = EDGE_CURVE ( 'NONE', #5374, #813, #680, .T. ) ;
#7987 = EDGE_LOOP ( 'NONE', ( #3025, #7306, #5320, #8060 ) ) ;
#7988 = DIRECTION ( 'NONE',  ( -0.000000000000000000, 0.000000000000000000, 1.000000000000000000 ) ) ;
#7989 =( CONVERSION_BASED_UNIT ( 'INCH', #3007 ) LENGTH_UNIT ( ) NAMED_UNIT ( #4994 ) );
#7990 = ORIENTED_EDGE ( 'NONE', *, *, #5350, .T. ) ;
#7991 = DIRECTION ( 'NONE',  ( 1.000000000000000000, 0.000000000000000000, 0.000000000000000000 ) ) ;
#7992 = CALENDAR_DATE ( 2026, 9, 10 ) ;
#7993 = DIRECTION ( 'NONE',  ( -0.000000000000000000, -0.000000000000000000, -1.000000000000000000 ) ) ;
#7994 = VERTEX_POINT ( 'NONE', #6910 ) ;
#7995 = ORIENTED_EDGE ( 'NONE', *, *, #1236, .F. ) ;
#7996 = LOCAL_TIME ( 14, 45, 32.00000000000000000, #7278 ) ;
#7997 = CARTESIAN_POINT ( 'NONE',  ( 6.067385397437120353, 0.2407432673787524013, -0.1849999999999999978 ) ) ;
#7998 = CYLINDRICAL_SURFACE ( 'NONE', #7932, 0.2515937209583817280 ) ;
#7999 = CARTESIAN_POINT ( 'NONE',  ( 6.000000000000001776, 0.000000000000000000, 0.1850000000000003586 ) ) ;
#8000 = COORDINATED_UNIVERSAL_TIME_OFFSET ( 0, 0, .AHEAD. ) ;
#8001 = DIRECTION ( 'NONE',  ( 0.000000000000000000, 0.000000000000000000, -1.000000000000000000 ) ) ;
#8002 = CARTESIAN_POINT ( 'NONE',  ( -4.790174522854136363, -3.094341753229061798, 0.000000000000000000 ) ) ;
#8003 = CIRCLE ( 'NONE', #2902, 0.2499999999999998057 ) ;
#8004 = ORIENTED_EDGE ( 'NONE', *, *, #6595, .F. ) ;
#8005 = CARTESIAN_POINT ( 'NONE',  ( 1.594422663808446217, 1.192243756349470551, 0.1923732503636950975 ) ) ;
#8006 =( GEOMETRIC_REPRESENTATION_CONTEXT ( 3 ) GLOBAL_UNCERTAINTY_ASSIGNED_CONTEXT ( ( #5973 ) ) GLOBAL_UNIT_ASSIGNED_CONTEXT ( ( #127, #7586, #4408 ) ) REPRESENTATION_CONTEXT ( 'NONE', 'WORKASPACE' ) );
#8007 = CARTESIAN_POINT ( 'NONE',  ( 2.056298385200680201, 0.7198786976815837457, -0.1250000000000000000 ) ) ;
#8008 = CC_DESIGN_SECURITY_CLASSIFICATION ( #1471, ( #1211 ) ) ;
#8009 = VECTOR ( 'NONE', #3003, 39.37007874015748143 ) ;
#8010 = FACE_OUTER_BOUND ( 'NONE', #3066, .T. ) ;
#8011 = CARTESIAN_POINT ( 'NONE',  ( 1.272999066882351205, 1.052213837524887508, -0.07009719302410664932 ) ) ;
#8012 = FACE_OUTER_BOUND ( 'NONE', #3909, .T. ) ;
#8013 = AXIS2_PLACEMENT_3D ( 'NONE', #1337, #1260, #5737 ) ;
#8014 = CARTESIAN_POINT ( 'NONE',  ( -6.110602001756019419, -1.404684638105634820, 0.2500000000000000000 ) ) ;
#8015 = AXIS2_PLACEMENT_3D ( 'NONE', #581, #6167, #463 ) ;
#8016 = CYLINDRICAL_SURFACE ( 'NONE', #192, 0.06250000000000000000 ) ;
#8017 = DIRECTION ( 'NONE',  ( 0.000000000000000000, -0.000000000000000000, 1.000000000000000000 ) ) ;
#8018 = CALENDAR_DATE ( 2026, 9, 10 ) ;
#8019 = EDGE_LOOP ( 'NONE', ( #65, #2676, #5820, #6517, #108 ) ) ;
#8020 = DIRECTION ( 'NONE',  ( 1.000000000000000000, 0.000000000000000000, 0.000000000000000000 ) ) ;
#8021 = DIRECTION ( 'NONE',  ( -0.000000000000000000, 1.000000000000000000, -0.000000000000000000 ) ) ;
#8022 = ORIENTED_EDGE ( 'NONE', *, *, #985, .T. ) ;
#8023 = FACE_OUTER_BOUND ( 'NONE', #184, .T. ) ;
#8024 = EDGE_CURVE ( 'NONE', #7415, #4011, #2373, .T. ) ;
#8025 = AXIS2_PLACEMENT_3D ( 'NONE', #4417, #6912, #1247 ) ;
#8026 = EDGE_CURVE ( 'NONE', #2111, #1048, #3945, .T. ) ;
#8027 = VECTOR ( 'NONE', #128, 39.37007874015748143 ) ;
#8028 = ORIENTED_EDGE ( 'NONE', *, *, #823, .T. ) ;
#8029 = DIRECTION ( 'NONE',  ( 1.000000000000000000, 0.000000000000000000, 0.000000000000000000 ) ) ;
#8030 = APPROVAL_PERSON_ORGANIZATION ( #2008, #5247, #3580 ) ;
#8031 = FACE_OUTER_BOUND ( 'NONE', #2169, .T. ) ;
#8032 = AXIS2_PLACEMENT_3D ( 'NONE', #5014, #1699, #6173 ) ;
#8033 = DATE_AND_TIME ( #7992, #4122 ) ;
#8034 = CYLINDRICAL_SURFACE ( 'NONE', #2416, 0.03200000000000003536 ) ;
#8035 = VECTOR ( 'NONE', #4585, 39.37007874015748143 ) ;
#8036 = AXIS2_PLACEMENT_3D ( 'NONE', #5495, #3655, #529 ) ;
#8037 = ORIENTED_EDGE ( 'NONE', *, *, #5634, .T. ) ;
#8038 = CARTESIAN_POINT ( 'NONE',  ( 0.2796912674003787513, -4.528516545235624413, 0.03199999999999999373 ) ) ;
#8039 = DIRECTION ( 'NONE',  ( 0.000000000000000000, 0.000000000000000000, -1.000000000000000000 ) ) ;
#8040 = CARTESIAN_POINT ( 'NONE',  ( 0.09071608944134439134, -0.4599287527268067777, 0.02334334155383705270 ) ) ;
#8041 = PERSON_AND_ORGANIZATION ( #4735, #6190 ) ;
#8042 = DIRECTION ( 'NONE',  ( 0.000000000000000000, 0.000000000000000000, -1.000000000000000000 ) ) ;
#8043 = FACE_OUTER_BOUND ( 'NONE', #4608, .T. ) ;
#8044 = TOROIDAL_SURFACE ( 'NONE', #3610, 0.1487499999999999933, 0.03125000000000000000 ) ;
#8045 = EDGE_LOOP ( 'NONE', ( #7710, #1738, #5149, #4235 ) ) ;
#8046 = CARTESIAN_POINT ( 'NONE',  ( -0.1255000000000000282, 1.536931732929928570E-17, 0.06300000000000000044 ) ) ;
#8047 = VERTEX_POINT ( 'NONE', #7677 ) ;
#8048 = DIRECTION ( 'NONE',  ( -0.000000000000000000, 0.000000000000000000, 1.000000000000000000 ) ) ;
#8049 = DIRECTION ( 'NONE',  ( 0.000000000000000000, -1.000000000000000000, 0.000000000000000000 ) ) ;
#8050 = LINE ( 'NONE', #444, #6632 ) ;
#8051 = CIRCLE ( 'NONE', #4534, 3.939999999999463487 ) ;
#8052 = ORIENTED_EDGE ( 'NONE', *, *, #168, .T. ) ;
#8053 = EDGE_LOOP ( 'NONE', ( #5968, #5458, #1732, #2255 ) ) ;
#8054 = CARTESIAN_POINT ( 'NONE',  ( 1.591124618940792157, 1.197007719324126640, 0.1929411818709917681 ) ) ;
#8055 = AXIS2_PLACEMENT_3D ( 'NONE', #6827, #1176, #2328 ) ;
#8056 = CIRCLE ( 'NONE', #4023, 0.2812500000000000555 ) ;
#8057 = CARTESIAN_POINT ( 'NONE',  ( 0.000000000000000000, 0.000000000000000000, 0.1100000000000000006 ) ) ;
#8058 = LINE ( 'NONE', #6239, #1269 ) ;
#8059 = PERSON_AND_ORGANIZATION_ROLE ( 'classification_officer' ) ;
#8060 = ORIENTED_EDGE ( 'NONE', *, *, #872, .F. ) ;
#8061 = CARTESIAN_POINT ( 'NONE',  ( -1.763177565995707630, 1.070083551578369763, -0.2959999999999997078 ) ) ;
#8062 = VECTOR ( 'NONE', #7901, 39.37007874015748854 ) ;
#8063 = AXIS2_PLACEMENT_3D ( 'NONE', #6136, #7917, #7443 ) ;
#8064 = DIRECTION ( 'NONE',  ( 0.7879377495398141029, 0.6157549048526801405, 0.000000000000000000 ) ) ;
#8065 = ORIENTED_EDGE ( 'NONE', *, *, #5694, .T. ) ;
#8066 = CARTESIAN_POINT ( 'NONE',  ( 1.723083782080649939, 1.395997476760423961, 0.1965221205739769994 ) ) ;
#8067 = AXIS2_PLACEMENT_3D ( 'NONE', #3125, #4925, #6929 ) ;
#8068 =( REPRESENTATION_RELATIONSHIP ('NONE','NONE', #3360, #5024 ) REPRESENTATION_RELATIONSHIP_WITH_TRANSFORMATION ( #5470 )SHAPE_REPRESENTATION_RELATIONSHIP( ) );
#8069 = ORIENTED_EDGE ( 'NONE', *, *, #5595, .F. ) ;
#8070 = CIRCLE ( 'NONE', #4679, 0.4060000000000000830 ) ;
#8071 = CARTESIAN_POINT ( 'NONE',  ( -0.04782642554762441683, -0.03125000000000000000, 0.000000000000000000 ) ) ;
#8072 = EDGE_CURVE ( 'NONE', #2236, #2877, #3910, .T. ) ;
#8073 = CARTESIAN_POINT ( 'NONE',  ( 1.571814533976804151, 1.273076930690908437, 0.2372021369714001904 ) ) ;
#8074 = CALENDAR_DATE ( 2026, 9, 10 ) ;
#8075 = FACE_OUTER_BOUND ( 'NONE', #1952, .T. ) ;
#8076 = ORIENTED_EDGE ( 'NONE', *, *, #8072, .T. ) ;
#8077 = DIRECTION ( 'NONE',  ( 0.000000000000000000, 0.000000000000000000, -1.000000000000000000 ) ) ;
#8078 = DIRECTION ( 'NONE',  ( -0.000000000000000000, -0.000000000000000000, 1.000000000000000000 ) ) ;
#8079 = EDGE_CURVE ( 'NONE', #5927, #7385, #6449, .T. ) ;
#8080 = UNCERTAINTY_MEASURE_WITH_UNIT (LENGTH_MEASURE( 1.000000000000000082E-05 ), #7387, 'distance_accuracy_value', 'NONE');
#8081 = EDGE_CURVE ( 'NONE', #19, #2657, #5268, .T. ) ;
#8082 = CARTESIAN_POINT ( 'NONE',  ( -0.1250000000000000000, 0.5625000000000000000, -0.03125000000000000000 ) ) ;
#8083 = DATE_AND_TIME ( #474, #543 ) ;
#8084 = CARTESIAN_POINT ( 'NONE',  ( 0.7739487307887357170, -0.3852760516983189110, 0.07449999999999999678 ) ) ;
#8085 = CARTESIAN_POINT ( 'NONE',  ( 1.530682660343759327, 1.858020273156397284, -0.04707677864884684399 ) ) ;
#8086 = EDGE_CURVE ( 'NONE', #1380, #1544, #5392, .T. ) ;
#8087 = ORIENTED_EDGE ( 'NONE', *, *, #131, .F. ) ;
#8088 = CARTESIAN_POINT ( 'NONE',  ( 1.645823524873871069, 1.331476452140092581, 0.2367343346927103520 ) ) ;
#8089 = APPROVAL ( #5457, 'UNSPECIFIED' ) ;
#8090 = EDGE_CURVE ( 'NONE', #2766, #4981, #3947, .T. ) ;
#8091 = EDGE_LOOP ( 'NONE', ( #7482, #935, #5988, #155 ) ) ;
#8092 = NEXT_ASSEMBLY_USAGE_OCCURRENCE ( 'NAUO1', ' ', ' ', #5402, #3498, $ ) ;
#8093 = NEXT_ASSEMBLY_USAGE_OCCURRENCE ( 'NAUO2', ' ', ' ', #5402, #7594, $ ) ;
#8094 = NEXT_ASSEMBLY_USAGE_OCCURRENCE ( 'NAUO3', ' ', ' ', #5402, #3600, $ ) ;
#8095 = NEXT_ASSEMBLY_USAGE_OCCURRENCE ( 'NAUO4', ' ', ' ', #5402, #830, $ ) ;
#8096 = NEXT_ASSEMBLY_USAGE_OCCURRENCE ( 'NAUO5', ' ', ' ', #5402, #172, $ ) ;
#8097 = NEXT_ASSEMBLY_USAGE_OCCURRENCE ( 'NAUO6', ' ', ' ', #5402, #6001, $ ) ;
#8098 = NEXT_ASSEMBLY_USAGE_OCCURRENCE ( 'NAUO7', ' ', ' ', #5402, #6001, $ ) ;
#8099 = NEXT_ASSEMBLY_USAGE_OCCURRENCE ( 'NAUO8', ' ', ' ', #3600, #5651, $ ) ;
#8100 = NEXT_ASSEMBLY_USAGE_OCCURRENCE ( 'NAUO9', ' ', ' ', #3600, #7247, $ ) ;
#8101 = COLOUR_RGB('Deep Blue', 0.66274510, 0.83137255, 0.94901961);
#8102 = FILL_AREA_STYLE_COLOUR('',#8101);
#8103 = FILL_AREA_STYLE('',(#8102));
#8104 = SURFACE_STYLE_FILL_AREA(#8103);
#8105 = SURFACE_SIDE_STYLE('',(#8104));
#8106 = SURFACE_STYLE_USAGE(.BOTH.,#8105);
#8107 = PRESENTATION_STYLE_ASSIGNMENT((#8106));
#8108 = COLOUR_RGB('Light Blue', 0.31764706, 0.68627451, 0.89019608);
#8109 = FILL_AREA_STYLE_COLOUR('',#8108);
#8110 = FILL_AREA_STYLE('',(#8109));
#8111 = SURFACE_STYLE_FILL_AREA(#8110);
#8112 = SURFACE_SIDE_STYLE('',(#8111));
#8113 = SURFACE_STYLE_USAGE(.BOTH.,#8112);
#8114 = PRESENTATION_STYLE_ASSIGNMENT((#8113));
#8115 = COLOUR_RGB('Sky Blue', 0.40784314, 0.44705882, 0.49803922);
#8116 = FILL_AREA_STYLE_COLOUR('',#8115);
#8117 = FILL_AREA_STYLE('',(#8116));
#8118 = SURFACE_STYLE_FILL_AREA(#8117);
#8119 = SURFACE_SIDE_STYLE('',(#8118));
#8120 = SURFACE_STYLE_USAGE(.BOTH.,#8119);
#8121 = PRESENTATION_STYLE_ASSIGNMENT((#8120));
#8122 = COLOUR_RGB('Slate Gray', 0.72549020, 0.75294118, 0.79215686);
#8123 = FILL_AREA_STYLE_COLOUR('',#8122);
#8124 = FILL_AREA_STYLE('',(#8123));
#8125 = SURFACE_STYLE_FILL_AREA(#8124);
#8126 = SURFACE_SIDE_STYLE('',(#8125));
#8127 = SURFACE_STYLE_USAGE(.BOTH.,#8126);
#8128 = PRESENTATION_STYLE_ASSIGNMENT((#8127));
#8129 = COLOUR_RGB('Light Gray', 0.08235294, 0.09019608, 0.10196078);
#8130 = FILL_AREA_STYLE_COLOUR('',#8129);
#8131 = FILL_AREA_STYLE('',(#8130));
#8132 = SURFACE_STYLE_FILL_AREA(#8131);
#8133 = SURFACE_SIDE_STYLE('',(#8132));
#8134 = SURFACE_STYLE_USAGE(.BOTH.,#8133);
#8135 = PRESENTATION_STYLE_ASSIGNMENT((#8134));
#8136 = COLOUR_RGB('Black', 0.09019608, 0.27058824, 0.51372549);
#8137 = FILL_AREA_STYLE_COLOUR('',#8136);
#8138 = FILL_AREA_STYLE('',(#8137));
#8139 = SURFACE_STYLE_FILL_AREA(#8138);
#8140 = SURFACE_SIDE_STYLE('',(#8139));
#8141 = SURFACE_STYLE_USAGE(.BOTH.,#8140);
#8142 = PRESENTATION_STYLE_ASSIGNMENT((#8141));
#8143 = STYLED_ITEM('',(#8121),#3593);
#8144 = MECHANICAL_DESIGN_GEOMETRIC_PRESENTATION_REPRESENTATION('',(#8143),#553);
#8145 = STYLED_ITEM('',(#8114),#6445);
#8146 = STYLED_ITEM('',(#8142),#6285);
#8147 = MECHANICAL_DESIGN_GEOMETRIC_PRESENTATION_REPRESENTATION('',(#8145,#8146),#5783);
#8148 = STYLED_ITEM('',(#8107),#6340);
#8149 = MECHANICAL_DESIGN_GEOMETRIC_PRESENTATION_REPRESENTATION('',(#8148),#1726);
#8150 = STYLED_ITEM('',(#8135),#3760);
#8151 = MECHANICAL_DESIGN_GEOMETRIC_PRESENTATION_REPRESENTATION('',(#8150),#2122);
#8152 = STYLED_ITEM('',(#8128),#3690);
#8153 = MECHANICAL_DESIGN_GEOMETRIC_PRESENTATION_REPRESENTATION('',(#8152),#2249);
#8154 = STYLED_ITEM('',(#8107),#869);
#8155 = MECHANICAL_DESIGN_GEOMETRIC_PRESENTATION_REPRESENTATION('',(#8154),#2771);
#8156 = STYLED_ITEM('',(#8114),#3575);
#8157 = MECHANICAL_DESIGN_GEOMETRIC_PRESENTATION_REPRESENTATION('',(#8156),#6058);
ENDSEC;
END-ISO-10303-21;
